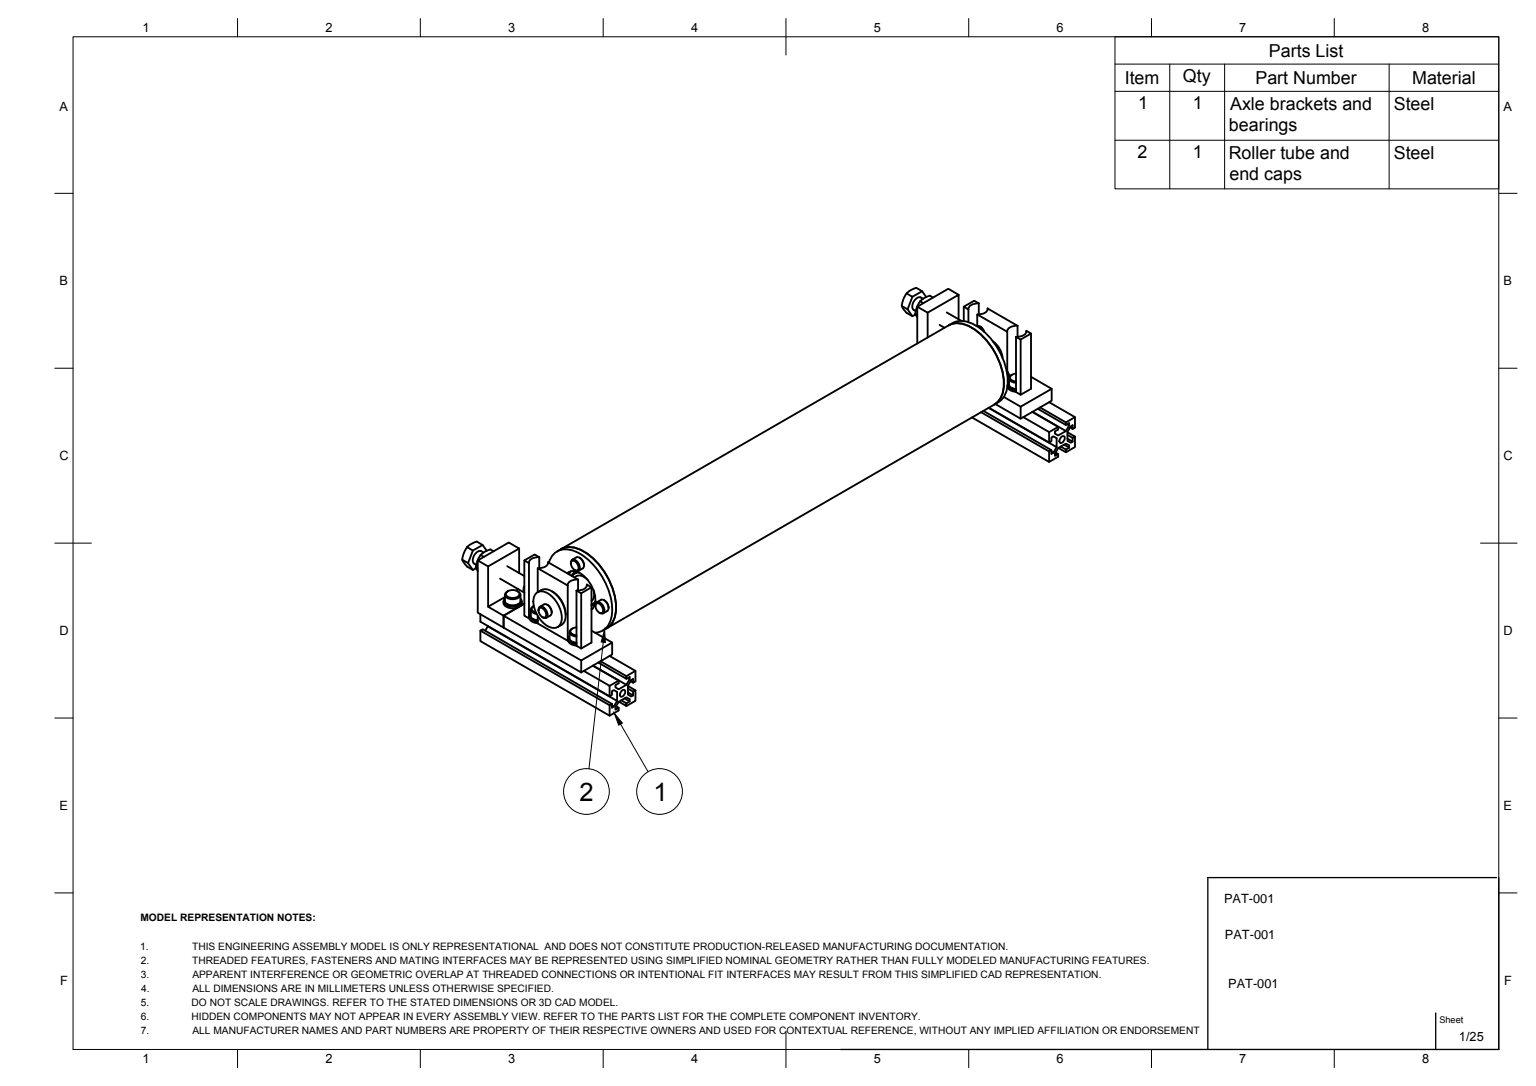
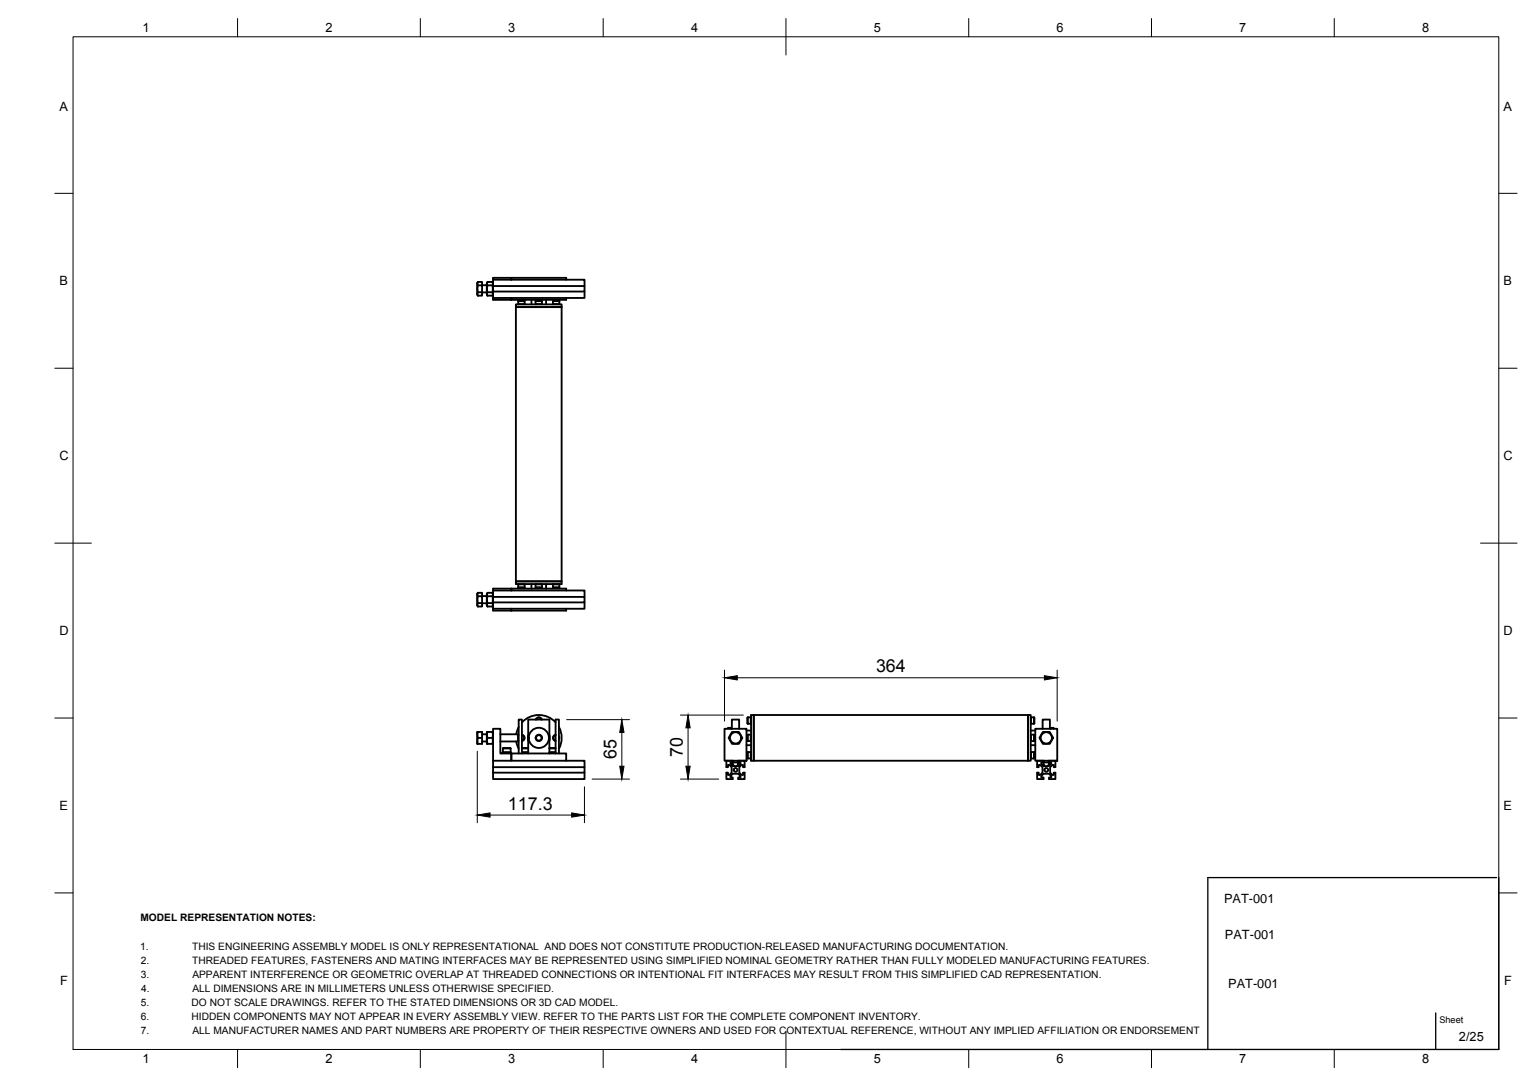
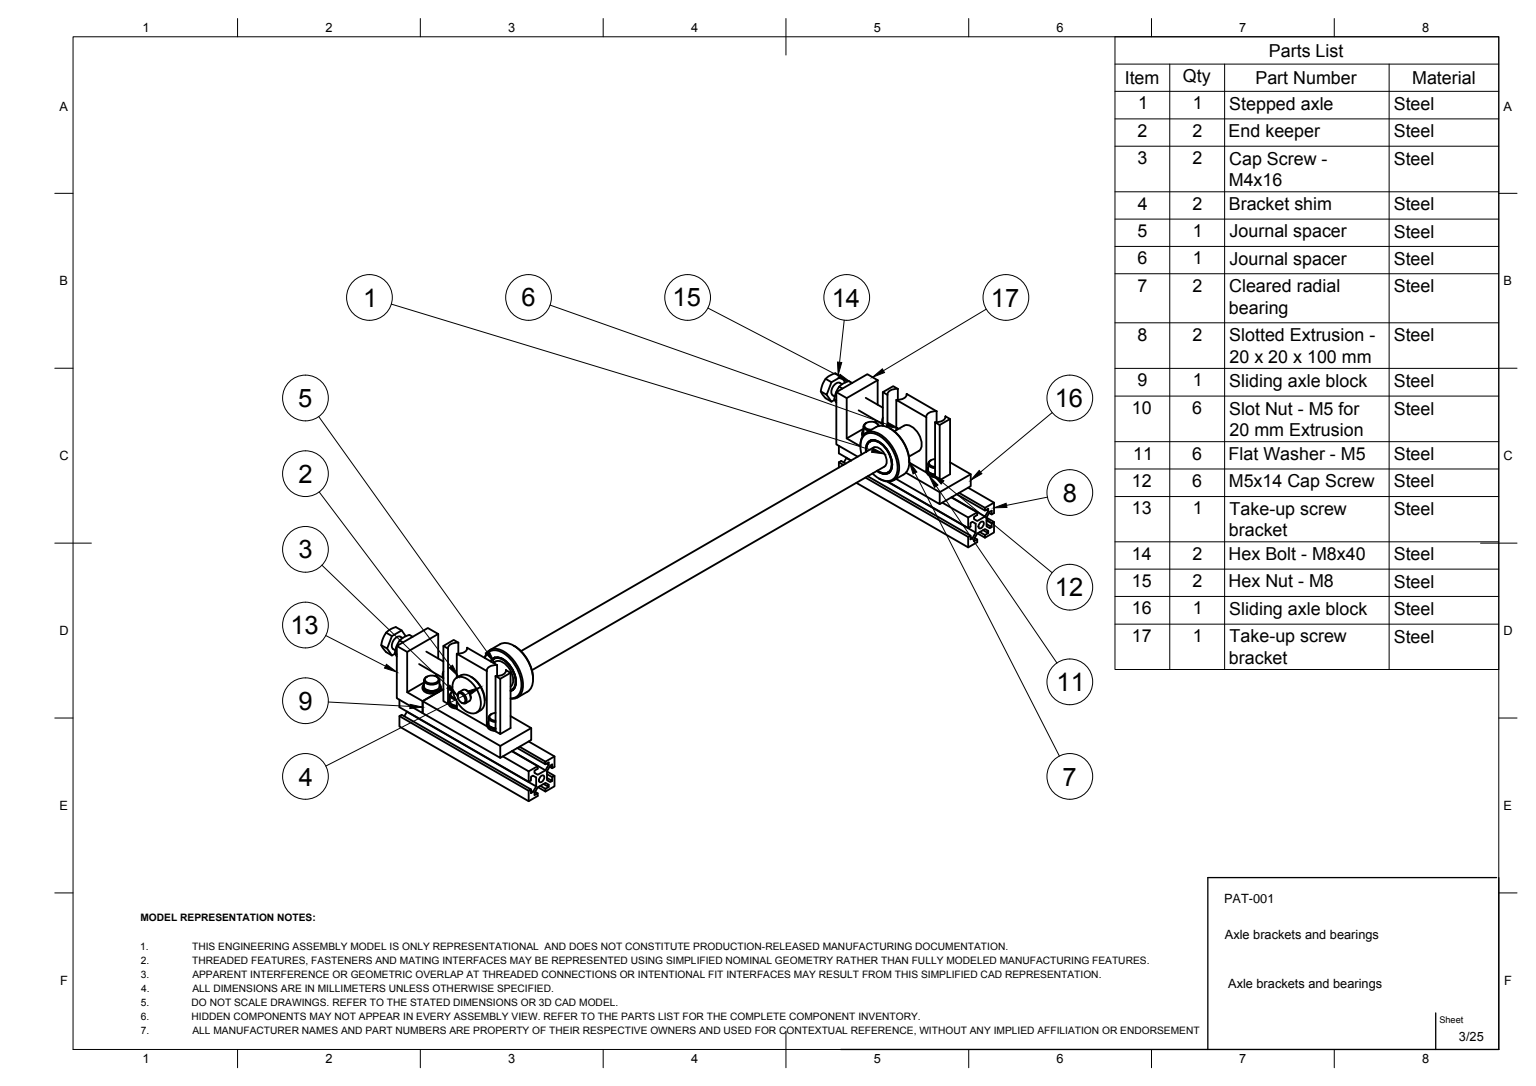
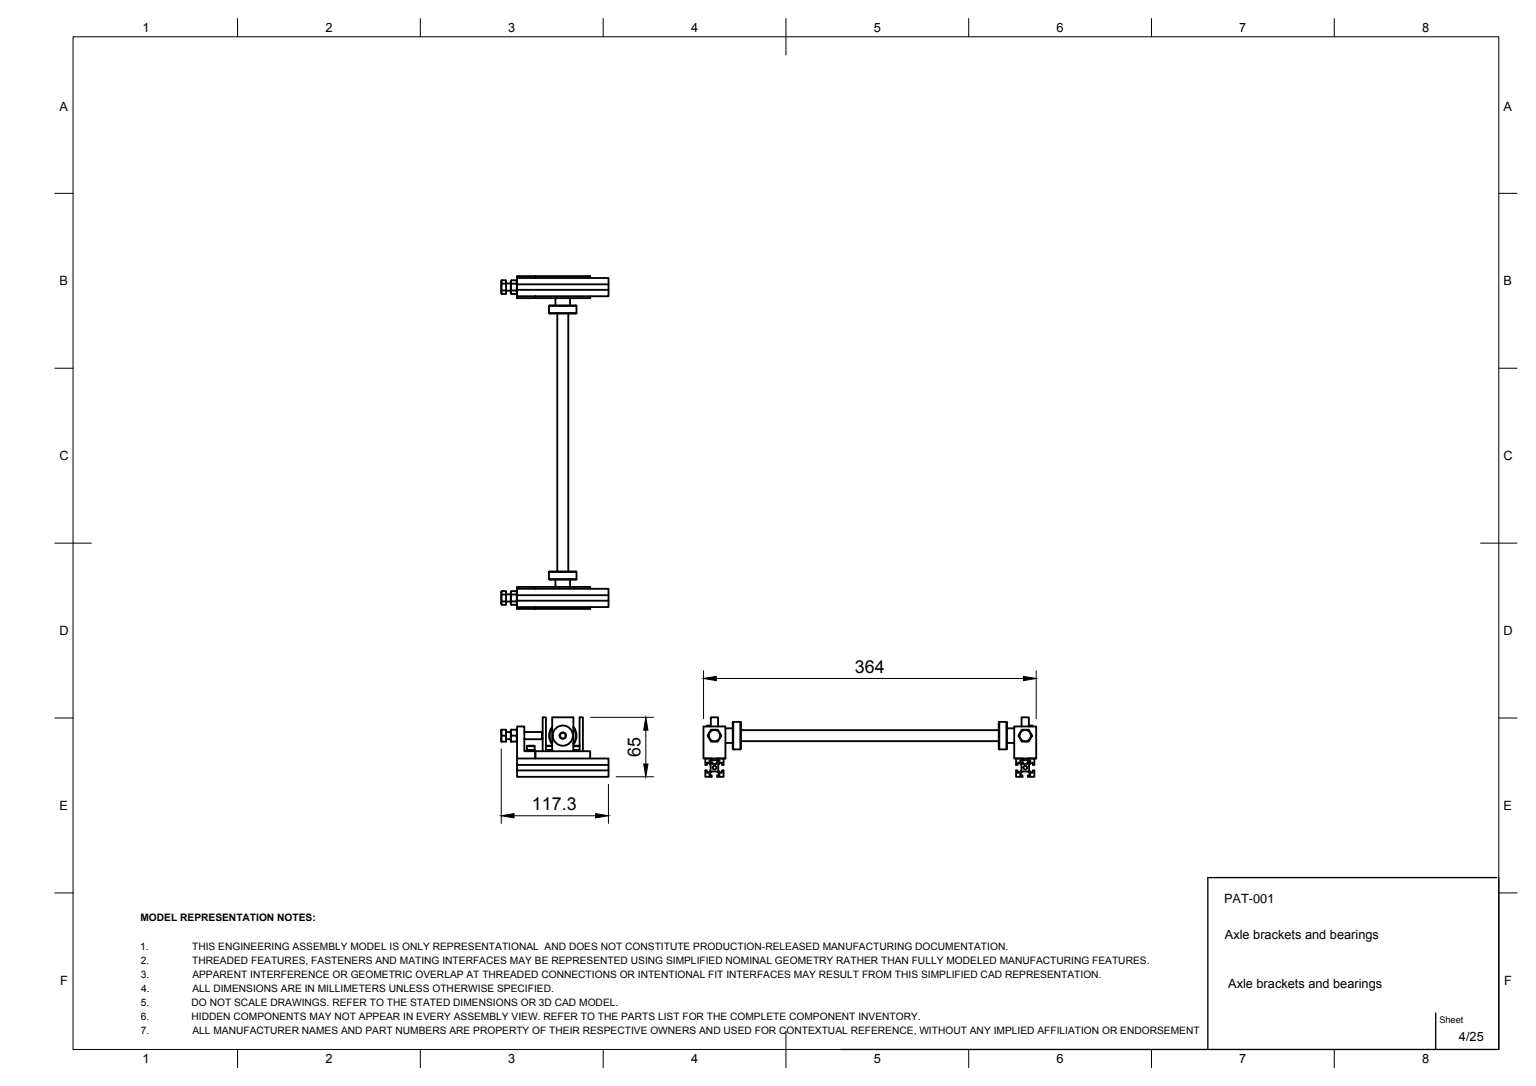
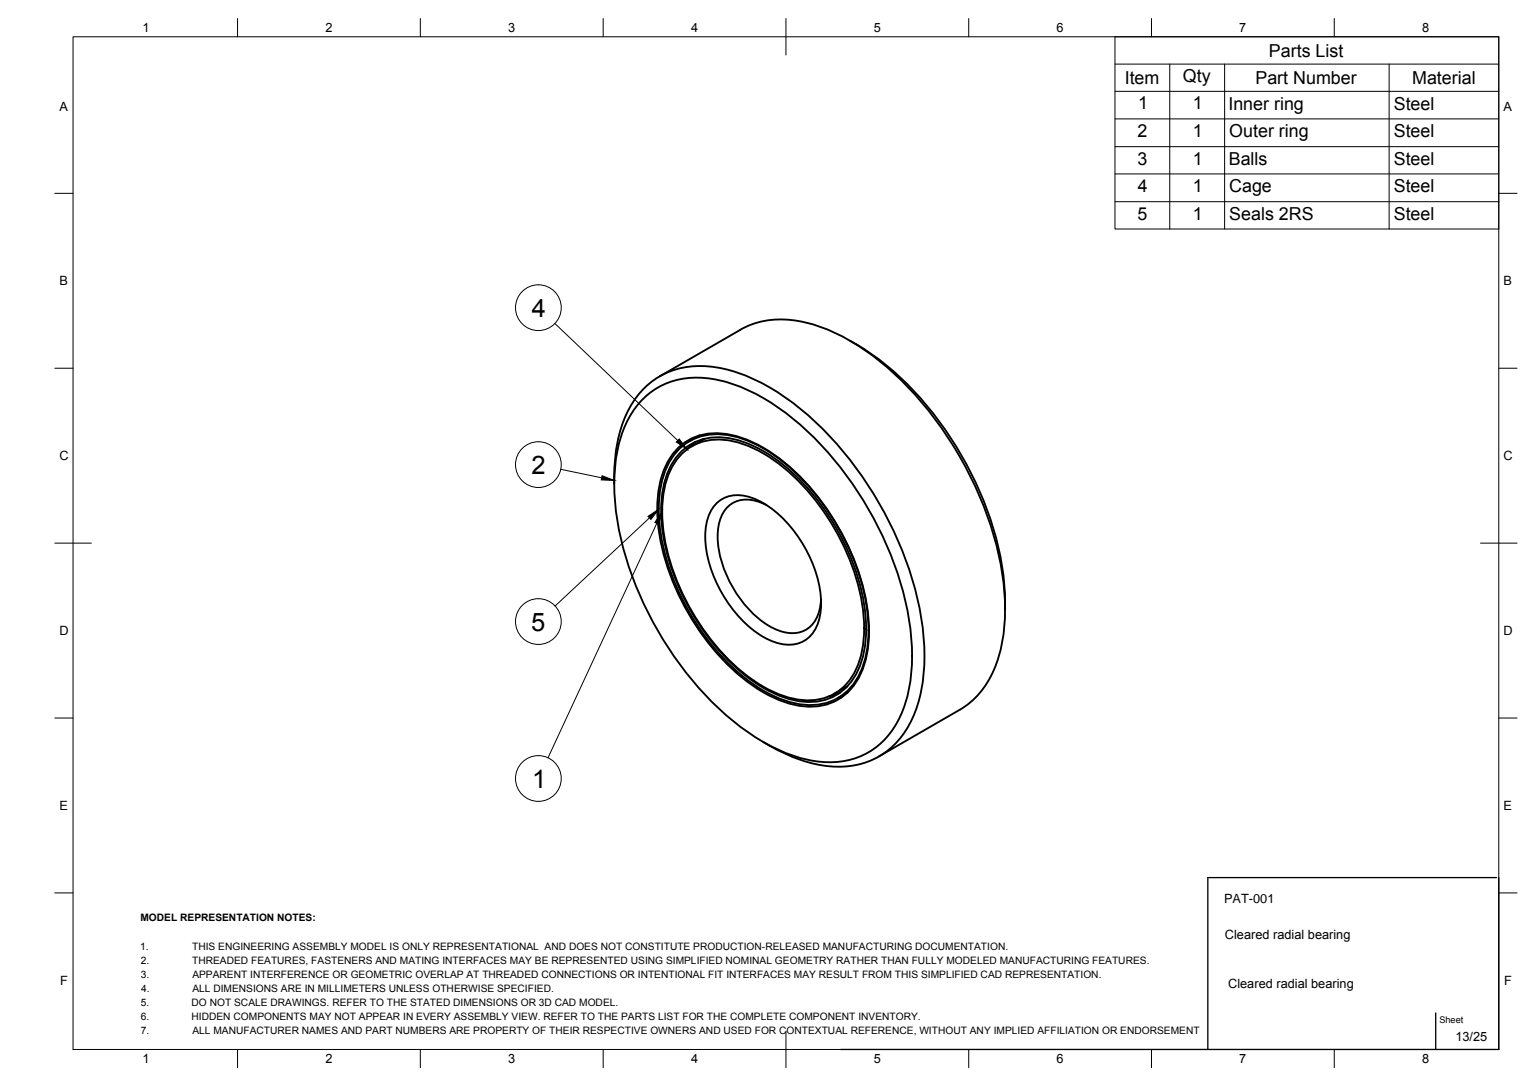
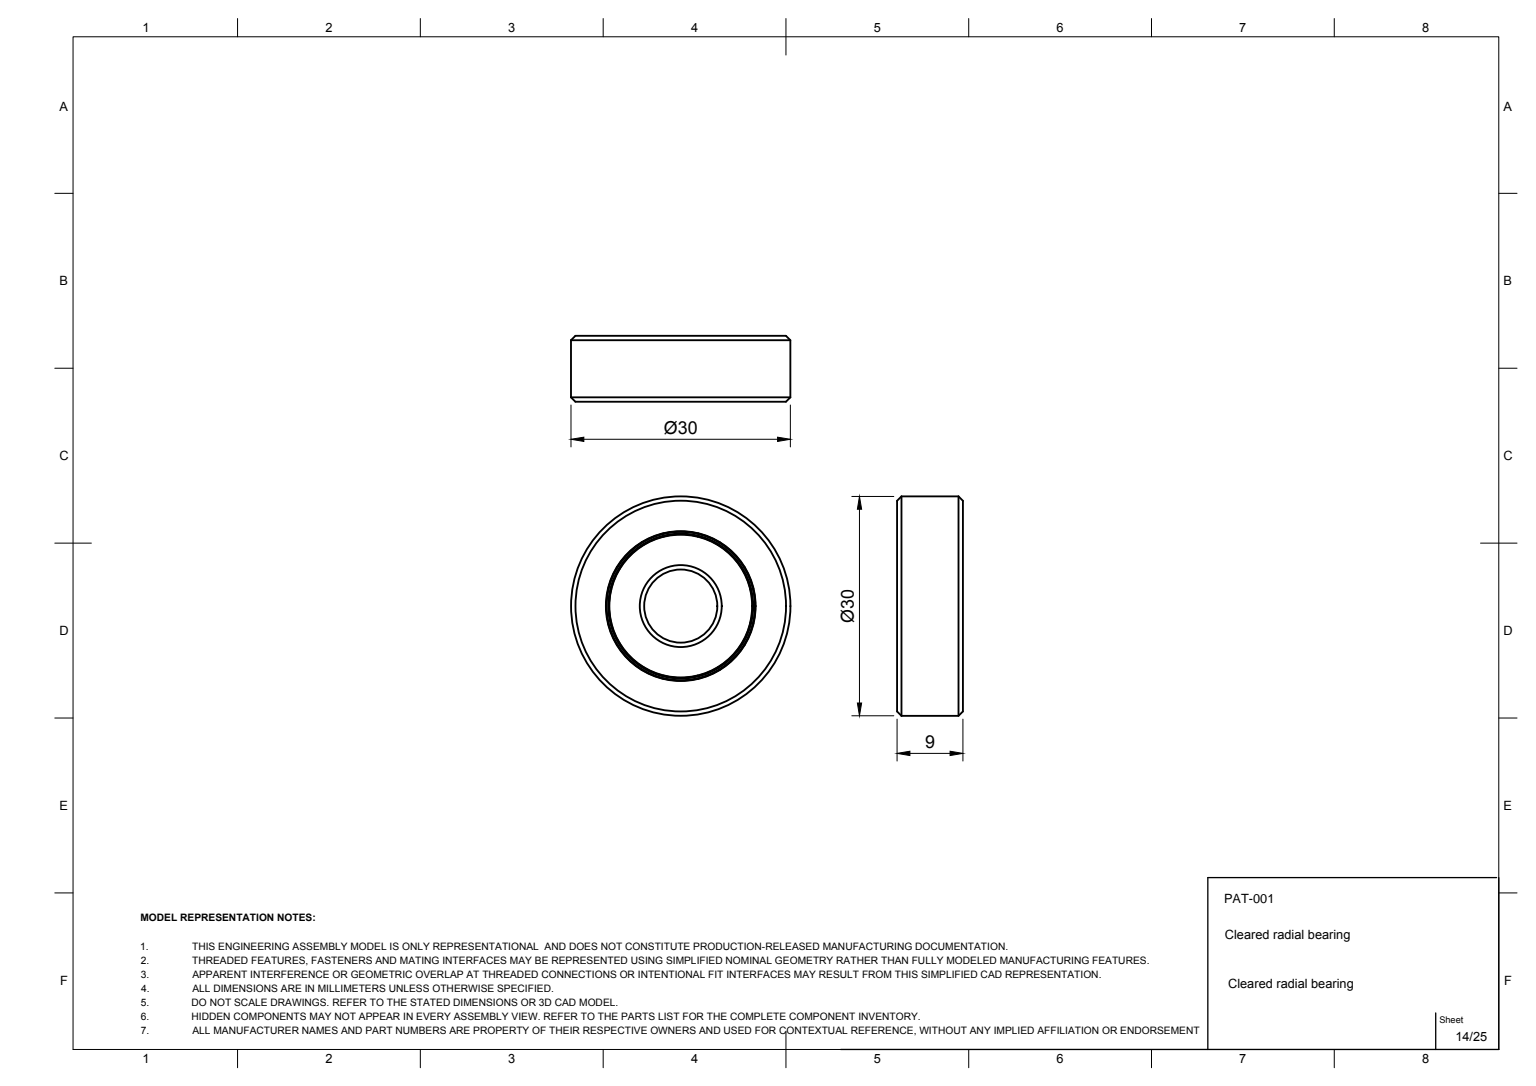
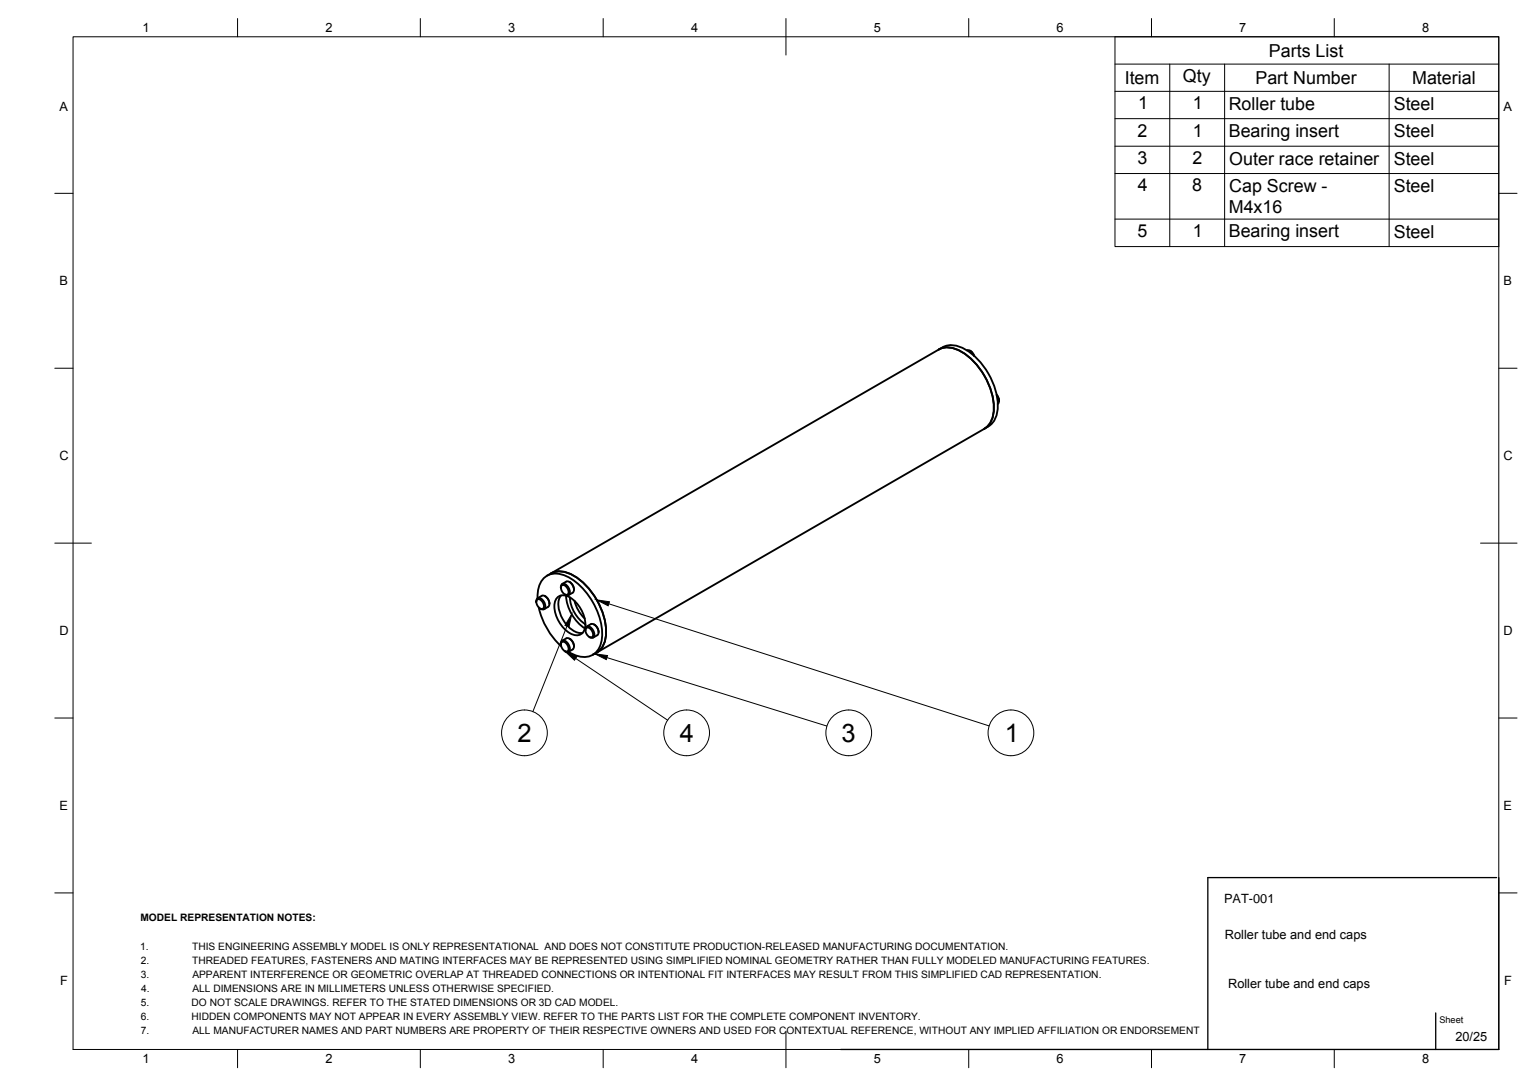
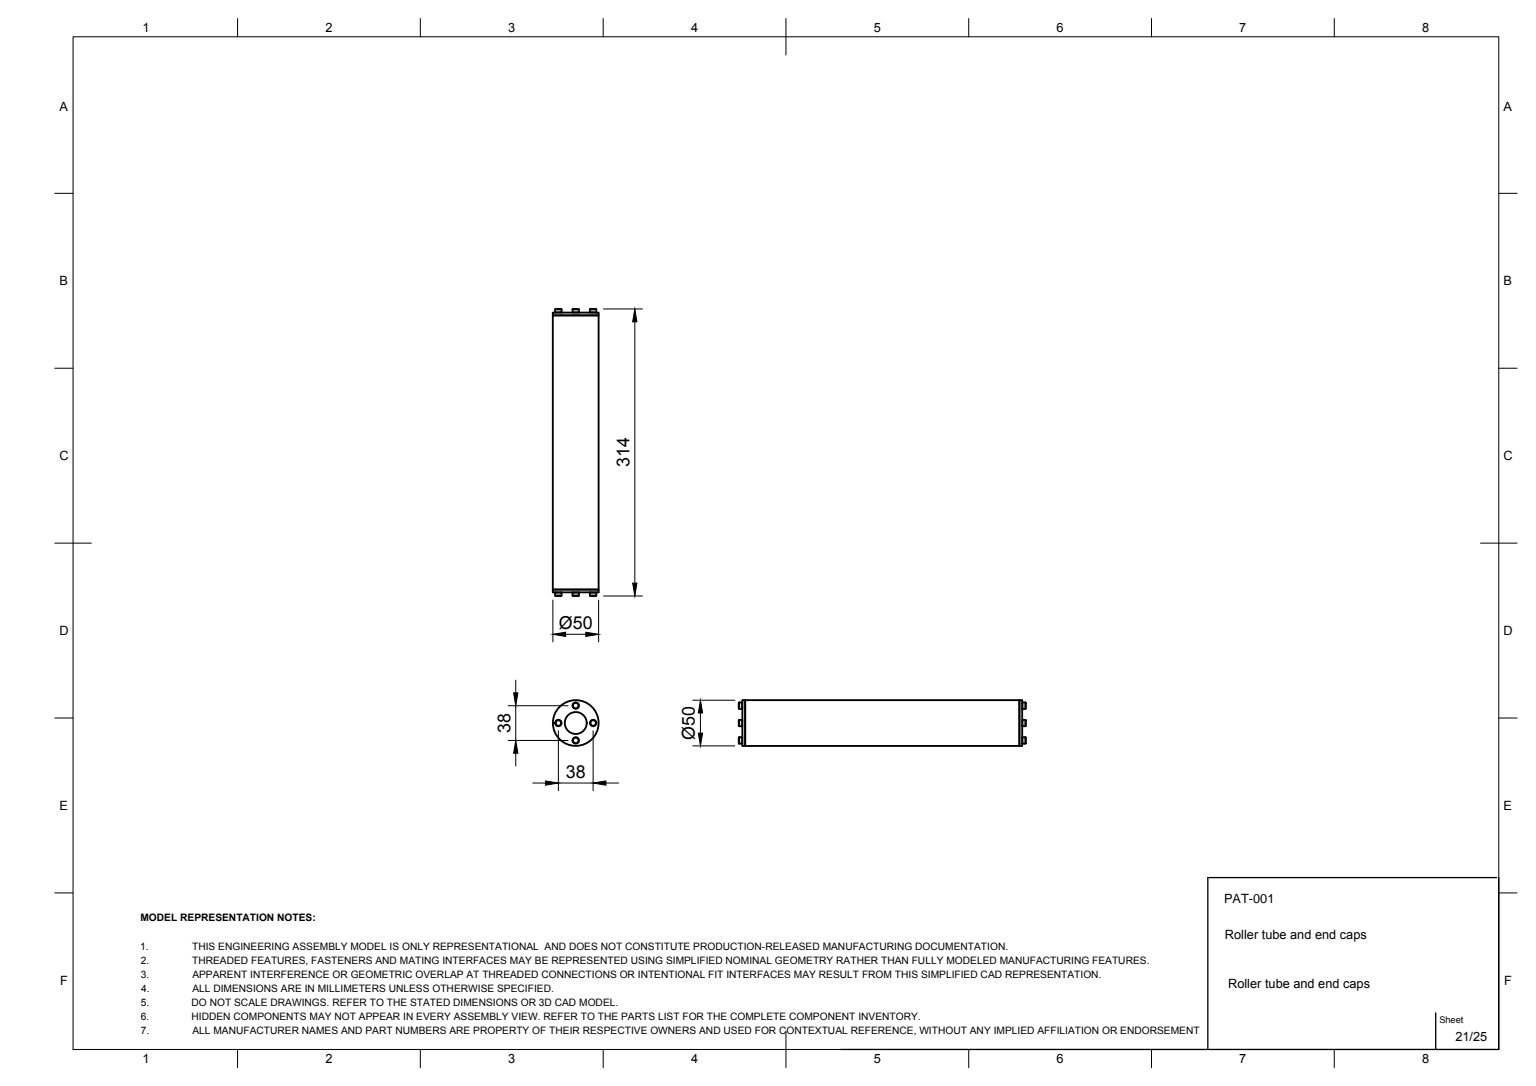
ISO-10303-21;
HEADER;
/* Generated by software containing ST-Developer
 * from STEP Tools, Inc. (www.steptools.com) 
 */

FILE_DESCRIPTION(
/* description */ ('PAT-001'),
/* implementation_level */ '2;1');

FILE_NAME(
/* name */ 'PAT-001',
/* time_stamp */ '2026-10-29T17:07:15-07:00',
/* author */ (''),
/* organization */ (''),
/* preprocessor_version */ 'ST-DEVELOPER v20.2',
/* originating_system */ 'Autodesk Translation Framework v15.17.0.0',
/* authorisation */ '');

FILE_SCHEMA (('AUTOMOTIVE_DESIGN { 1 0 10303 214 3 1 1 }'));
ENDSEC;

DATA;
#10=MECHANICAL_DESIGN_GEOMETRIC_PRESENTATION_REPRESENTATION('',(#373,#374,
#375,#376,#377,#378,#379,#380,#381,#382,#383,#384,#385,#386,#387,#388,#389,
#390,#391,#392,#393,#394,#395,#396,#397,#398,#399,#400,#401,#402,#403,#404,
#405),#9622);
#11=(
BOUNDED_CURVE()
B_SPLINE_CURVE(2,(#9167,#9168,#9169),.UNSPECIFIED.,.F.,.F.)
B_SPLINE_CURVE_WITH_KNOTS((3,3),(0.14973948338295,0.97160236658079),
 .UNSPECIFIED.)
CURVE()
GEOMETRIC_REPRESENTATION_ITEM()
RATIONAL_B_SPLINE_CURVE((1.07140024848292,1.23714644374248,1.07140024848292))
REPRESENTATION_ITEM('')
);
#12=(
BOUNDED_CURVE()
B_SPLINE_CURVE(2,(#9171,#9172,#9173),.UNSPECIFIED.,.F.,.F.)
B_SPLINE_CURVE_WITH_KNOTS((3,3),(0.14973948338295,0.97160236658079),
 .UNSPECIFIED.)
CURVE()
GEOMETRIC_REPRESENTATION_ITEM()
RATIONAL_B_SPLINE_CURVE((1.07140024848292,1.23714644374248,1.07140024848292))
REPRESENTATION_ITEM('')
);
#13=(
BOUNDED_CURVE()
B_SPLINE_CURVE(2,(#9175,#9176,#9177),.UNSPECIFIED.,.F.,.F.)
B_SPLINE_CURVE_WITH_KNOTS((3,3),(0.14973948338295,0.97160236658079),
 .UNSPECIFIED.)
CURVE()
GEOMETRIC_REPRESENTATION_ITEM()
RATIONAL_B_SPLINE_CURVE((1.07140024848292,1.23714644374248,1.07140024848292))
REPRESENTATION_ITEM('')
);
#14=(
BOUNDED_CURVE()
B_SPLINE_CURVE(2,(#9179,#9180,#9181),.UNSPECIFIED.,.F.,.F.)
B_SPLINE_CURVE_WITH_KNOTS((3,3),(0.149739483382949,0.971602366580789),
 .UNSPECIFIED.)
CURVE()
GEOMETRIC_REPRESENTATION_ITEM()
RATIONAL_B_SPLINE_CURVE((1.07140024848292,1.23714644374248,1.07140024848292))
REPRESENTATION_ITEM('')
);
#15=(
BOUNDED_CURVE()
B_SPLINE_CURVE(2,(#9183,#9184,#9185),.UNSPECIFIED.,.F.,.F.)
B_SPLINE_CURVE_WITH_KNOTS((3,3),(0.14973948338295,0.971602366580789),
 .UNSPECIFIED.)
CURVE()
GEOMETRIC_REPRESENTATION_ITEM()
RATIONAL_B_SPLINE_CURVE((1.07140024848292,1.23714644374248,1.07140024848292))
REPRESENTATION_ITEM('')
);
#16=(
BOUNDED_CURVE()
B_SPLINE_CURVE(2,(#9186,#9187,#9188),.UNSPECIFIED.,.F.,.F.)
B_SPLINE_CURVE_WITH_KNOTS((3,3),(0.14973948338295,0.97160236658079),
 .UNSPECIFIED.)
CURVE()
GEOMETRIC_REPRESENTATION_ITEM()
RATIONAL_B_SPLINE_CURVE((1.07140024848292,1.23714644374248,1.07140024848292))
REPRESENTATION_ITEM('')
);
#17=(
BOUNDED_CURVE()
B_SPLINE_CURVE(2,(#9219,#9220,#9221),.UNSPECIFIED.,.F.,.F.)
B_SPLINE_CURVE_WITH_KNOTS((3,3),(0.14973948338295,0.97160236658079),
 .UNSPECIFIED.)
CURVE()
GEOMETRIC_REPRESENTATION_ITEM()
RATIONAL_B_SPLINE_CURVE((1.07140024848292,1.23714644374248,1.07140024848292))
REPRESENTATION_ITEM('')
);
#18=(
BOUNDED_CURVE()
B_SPLINE_CURVE(2,(#9223,#9224,#9225),.UNSPECIFIED.,.F.,.F.)
B_SPLINE_CURVE_WITH_KNOTS((3,3),(0.14973948338295,0.971602366580789),
 .UNSPECIFIED.)
CURVE()
GEOMETRIC_REPRESENTATION_ITEM()
RATIONAL_B_SPLINE_CURVE((1.07140024848292,1.23714644374248,1.07140024848292))
REPRESENTATION_ITEM('')
);
#19=(
BOUNDED_CURVE()
B_SPLINE_CURVE(2,(#9230,#9231,#9232),.UNSPECIFIED.,.F.,.F.)
B_SPLINE_CURVE_WITH_KNOTS((3,3),(0.14973948338295,0.97160236658079),
 .UNSPECIFIED.)
CURVE()
GEOMETRIC_REPRESENTATION_ITEM()
RATIONAL_B_SPLINE_CURVE((1.07140024848292,1.23714644374248,1.07140024848292))
REPRESENTATION_ITEM('')
);
#20=(
BOUNDED_CURVE()
B_SPLINE_CURVE(2,(#9234,#9235,#9236),.UNSPECIFIED.,.F.,.F.)
B_SPLINE_CURVE_WITH_KNOTS((3,3),(0.14973948338295,0.97160236658079),
 .UNSPECIFIED.)
CURVE()
GEOMETRIC_REPRESENTATION_ITEM()
RATIONAL_B_SPLINE_CURVE((1.07140024848292,1.23714644374248,1.07140024848292))
REPRESENTATION_ITEM('')
);
#21=(
BOUNDED_CURVE()
B_SPLINE_CURVE(2,(#9238,#9239,#9240),.UNSPECIFIED.,.F.,.F.)
B_SPLINE_CURVE_WITH_KNOTS((3,3),(0.14973948338295,0.971602366580789),
 .UNSPECIFIED.)
CURVE()
GEOMETRIC_REPRESENTATION_ITEM()
RATIONAL_B_SPLINE_CURVE((1.07140024848292,1.23714644374248,1.07140024848292))
REPRESENTATION_ITEM('')
);
#22=(
BOUNDED_CURVE()
B_SPLINE_CURVE(2,(#9241,#9242,#9243),.UNSPECIFIED.,.F.,.F.)
B_SPLINE_CURVE_WITH_KNOTS((3,3),(0.14973948338295,0.97160236658079),
 .UNSPECIFIED.)
CURVE()
GEOMETRIC_REPRESENTATION_ITEM()
RATIONAL_B_SPLINE_CURVE((1.07140024848292,1.23714644374248,1.07140024848292))
REPRESENTATION_ITEM('')
);
#23=(
BOUNDED_CURVE()
B_SPLINE_CURVE(2,(#9250,#9251,#9252),.UNSPECIFIED.,.F.,.F.)
B_SPLINE_CURVE_WITH_KNOTS((3,3),(0.14973948338295,0.97160236658079),
 .UNSPECIFIED.)
CURVE()
GEOMETRIC_REPRESENTATION_ITEM()
RATIONAL_B_SPLINE_CURVE((1.07140024848292,1.23714644374248,1.07140024848292))
REPRESENTATION_ITEM('')
);
#24=(
BOUNDED_CURVE()
B_SPLINE_CURVE(2,(#9254,#9255,#9256),.UNSPECIFIED.,.F.,.F.)
B_SPLINE_CURVE_WITH_KNOTS((3,3),(0.14973948338295,0.97160236658079),
 .UNSPECIFIED.)
CURVE()
GEOMETRIC_REPRESENTATION_ITEM()
RATIONAL_B_SPLINE_CURVE((1.07140024848292,1.23714644374248,1.07140024848292))
REPRESENTATION_ITEM('')
);
#25=(
BOUNDED_CURVE()
B_SPLINE_CURVE(2,(#9258,#9259,#9260),.UNSPECIFIED.,.F.,.F.)
B_SPLINE_CURVE_WITH_KNOTS((3,3),(0.14973948338295,0.971602366580789),
 .UNSPECIFIED.)
CURVE()
GEOMETRIC_REPRESENTATION_ITEM()
RATIONAL_B_SPLINE_CURVE((1.07140024848292,1.23714644374248,1.07140024848292))
REPRESENTATION_ITEM('')
);
#26=(
BOUNDED_CURVE()
B_SPLINE_CURVE(2,(#9262,#9263,#9264),.UNSPECIFIED.,.F.,.F.)
B_SPLINE_CURVE_WITH_KNOTS((3,3),(0.14973948338295,0.97160236658079),
 .UNSPECIFIED.)
CURVE()
GEOMETRIC_REPRESENTATION_ITEM()
RATIONAL_B_SPLINE_CURVE((1.07140024848292,1.23714644374248,1.07140024848292))
REPRESENTATION_ITEM('')
);
#27=(
BOUNDED_CURVE()
B_SPLINE_CURVE(2,(#9266,#9267,#9268),.UNSPECIFIED.,.F.,.F.)
B_SPLINE_CURVE_WITH_KNOTS((3,3),(0.14973948338295,0.97160236658079),
 .UNSPECIFIED.)
CURVE()
GEOMETRIC_REPRESENTATION_ITEM()
RATIONAL_B_SPLINE_CURVE((1.07140024848292,1.23714644374248,1.07140024848292))
REPRESENTATION_ITEM('')
);
#28=(
BOUNDED_CURVE()
B_SPLINE_CURVE(2,(#9269,#9270,#9271),.UNSPECIFIED.,.F.,.F.)
B_SPLINE_CURVE_WITH_KNOTS((3,3),(0.14973948338295,0.971602366580789),
 .UNSPECIFIED.)
CURVE()
GEOMETRIC_REPRESENTATION_ITEM()
RATIONAL_B_SPLINE_CURVE((1.07140024848292,1.23714644374248,1.07140024848292))
REPRESENTATION_ITEM('')
);
#29=ORIENTED_CLOSED_SHELL('',*,#5223,.F.);
#30=ORIENTED_CLOSED_SHELL('',*,#5232,.F.);
#31=BREP_WITH_VOIDS('Body1',#5224,(#29));
#32=BREP_WITH_VOIDS('Body1',#5231,(#30));
#33=ELLIPSE('',#5863,0.299389011154384,0.2117);
#34=ELLIPSE('',#5868,0.299389011154384,0.2117);
#35=ITEM_DEFINED_TRANSFORMATION($,$,#5570,#5698);
#36=ITEM_DEFINED_TRANSFORMATION($,$,#5590,#5699);
#37=ITEM_DEFINED_TRANSFORMATION($,$,#5610,#5700);
#38=ITEM_DEFINED_TRANSFORMATION($,$,#5627,#5701);
#39=ITEM_DEFINED_TRANSFORMATION($,$,#5681,#5702);
#40=ITEM_DEFINED_TRANSFORMATION($,$,#5511,#6053);
#41=ITEM_DEFINED_TRANSFORMATION($,$,#5533,#6054);
#42=ITEM_DEFINED_TRANSFORMATION($,$,#5542,#6055);
#43=ITEM_DEFINED_TRANSFORMATION($,$,#5551,#6056);
#44=ITEM_DEFINED_TRANSFORMATION($,$,#5551,#6057);
#45=ITEM_DEFINED_TRANSFORMATION($,$,#6027,#6058);
#46=ITEM_DEFINED_TRANSFORMATION($,$,#6027,#6059);
#47=ITEM_DEFINED_TRANSFORMATION($,$,#5560,#6060);
#48=ITEM_DEFINED_TRANSFORMATION($,$,#5560,#6061);
#49=ITEM_DEFINED_TRANSFORMATION($,$,#5569,#6062);
#50=ITEM_DEFINED_TRANSFORMATION($,$,#5569,#6063);
#51=ITEM_DEFINED_TRANSFORMATION($,$,#5703,#6064);
#52=ITEM_DEFINED_TRANSFORMATION($,$,#5742,#6065);
#53=ITEM_DEFINED_TRANSFORMATION($,$,#5757,#6066);
#54=ITEM_DEFINED_TRANSFORMATION($,$,#5796,#6067);
#55=ITEM_DEFINED_TRANSFORMATION($,$,#5811,#6068);
#56=ITEM_DEFINED_TRANSFORMATION($,$,#5861,#6069);
#57=ITEM_DEFINED_TRANSFORMATION($,$,#5878,#6070);
#58=ITEM_DEFINED_TRANSFORMATION($,$,#5889,#6071);
#59=ITEM_DEFINED_TRANSFORMATION($,$,#5861,#6072);
#60=ITEM_DEFINED_TRANSFORMATION($,$,#5878,#6073);
#61=ITEM_DEFINED_TRANSFORMATION($,$,#5889,#6074);
#62=ITEM_DEFINED_TRANSFORMATION($,$,#5861,#6075);
#63=ITEM_DEFINED_TRANSFORMATION($,$,#5878,#6076);
#64=ITEM_DEFINED_TRANSFORMATION($,$,#5889,#6077);
#65=ITEM_DEFINED_TRANSFORMATION($,$,#5913,#6078);
#66=ITEM_DEFINED_TRANSFORMATION($,$,#5930,#6079);
#67=ITEM_DEFINED_TRANSFORMATION($,$,#5811,#6080);
#68=ITEM_DEFINED_TRANSFORMATION($,$,#5861,#6081);
#69=ITEM_DEFINED_TRANSFORMATION($,$,#5878,#6082);
#70=ITEM_DEFINED_TRANSFORMATION($,$,#5889,#6083);
#71=ITEM_DEFINED_TRANSFORMATION($,$,#5861,#6084);
#72=ITEM_DEFINED_TRANSFORMATION($,$,#5878,#6085);
#73=ITEM_DEFINED_TRANSFORMATION($,$,#5889,#6086);
#74=ITEM_DEFINED_TRANSFORMATION($,$,#5861,#6087);
#75=ITEM_DEFINED_TRANSFORMATION($,$,#5878,#6088);
#76=ITEM_DEFINED_TRANSFORMATION($,$,#5889,#6089);
#77=ITEM_DEFINED_TRANSFORMATION($,$,#5913,#6090);
#78=ITEM_DEFINED_TRANSFORMATION($,$,#5930,#6091);
#79=ITEM_DEFINED_TRANSFORMATION($,$,#5947,#6092);
#80=ITEM_DEFINED_TRANSFORMATION($,$,#5972,#6093);
#81=ITEM_DEFINED_TRANSFORMATION($,$,#5997,#6094);
#82=ITEM_DEFINED_TRANSFORMATION($,$,#6006,#6095);
#83=ITEM_DEFINED_TRANSFORMATION($,$,#6027,#6096);
#84=ITEM_DEFINED_TRANSFORMATION($,$,#6027,#6097);
#85=ITEM_DEFINED_TRANSFORMATION($,$,#6027,#6098);
#86=ITEM_DEFINED_TRANSFORMATION($,$,#6027,#6099);
#87=ITEM_DEFINED_TRANSFORMATION($,$,#6006,#6100);
#88=ITEM_DEFINED_TRANSFORMATION($,$,#6027,#6101);
#89=ITEM_DEFINED_TRANSFORMATION($,$,#6027,#6102);
#90=ITEM_DEFINED_TRANSFORMATION($,$,#6027,#6103);
#91=ITEM_DEFINED_TRANSFORMATION($,$,#6027,#6104);
#92=ITEM_DEFINED_TRANSFORMATION($,$,#5510,#6105);
#93=ITEM_DEFINED_TRANSFORMATION($,$,#5946,#6106);
#94=(
REPRESENTATION_RELATIONSHIP($,$,#9752,#9751)
REPRESENTATION_RELATIONSHIP_WITH_TRANSFORMATION(#35)
SHAPE_REPRESENTATION_RELATIONSHIP()
);
#95=(
REPRESENTATION_RELATIONSHIP($,$,#9753,#9751)
REPRESENTATION_RELATIONSHIP_WITH_TRANSFORMATION(#36)
SHAPE_REPRESENTATION_RELATIONSHIP()
);
#96=(
REPRESENTATION_RELATIONSHIP($,$,#9754,#9751)
REPRESENTATION_RELATIONSHIP_WITH_TRANSFORMATION(#37)
SHAPE_REPRESENTATION_RELATIONSHIP()
);
#97=(
REPRESENTATION_RELATIONSHIP($,$,#9755,#9751)
REPRESENTATION_RELATIONSHIP_WITH_TRANSFORMATION(#38)
SHAPE_REPRESENTATION_RELATIONSHIP()
);
#98=(
REPRESENTATION_RELATIONSHIP($,$,#9756,#9751)
REPRESENTATION_RELATIONSHIP_WITH_TRANSFORMATION(#39)
SHAPE_REPRESENTATION_RELATIONSHIP()
);
#99=(
REPRESENTATION_RELATIONSHIP($,$,#9746,#9745)
REPRESENTATION_RELATIONSHIP_WITH_TRANSFORMATION(#40)
SHAPE_REPRESENTATION_RELATIONSHIP()
);
#100=(
REPRESENTATION_RELATIONSHIP($,$,#9747,#9745)
REPRESENTATION_RELATIONSHIP_WITH_TRANSFORMATION(#41)
SHAPE_REPRESENTATION_RELATIONSHIP()
);
#101=(
REPRESENTATION_RELATIONSHIP($,$,#9748,#9745)
REPRESENTATION_RELATIONSHIP_WITH_TRANSFORMATION(#42)
SHAPE_REPRESENTATION_RELATIONSHIP()
);
#102=(
REPRESENTATION_RELATIONSHIP($,$,#9749,#9745)
REPRESENTATION_RELATIONSHIP_WITH_TRANSFORMATION(#43)
SHAPE_REPRESENTATION_RELATIONSHIP()
);
#103=(
REPRESENTATION_RELATIONSHIP($,$,#9749,#9745)
REPRESENTATION_RELATIONSHIP_WITH_TRANSFORMATION(#44)
SHAPE_REPRESENTATION_RELATIONSHIP()
);
#104=(
REPRESENTATION_RELATIONSHIP($,$,#9772,#9745)
REPRESENTATION_RELATIONSHIP_WITH_TRANSFORMATION(#45)
SHAPE_REPRESENTATION_RELATIONSHIP()
);
#105=(
REPRESENTATION_RELATIONSHIP($,$,#9772,#9745)
REPRESENTATION_RELATIONSHIP_WITH_TRANSFORMATION(#46)
SHAPE_REPRESENTATION_RELATIONSHIP()
);
#106=(
REPRESENTATION_RELATIONSHIP($,$,#9750,#9745)
REPRESENTATION_RELATIONSHIP_WITH_TRANSFORMATION(#47)
SHAPE_REPRESENTATION_RELATIONSHIP()
);
#107=(
REPRESENTATION_RELATIONSHIP($,$,#9750,#9745)
REPRESENTATION_RELATIONSHIP_WITH_TRANSFORMATION(#48)
SHAPE_REPRESENTATION_RELATIONSHIP()
);
#108=(
REPRESENTATION_RELATIONSHIP($,$,#9751,#9745)
REPRESENTATION_RELATIONSHIP_WITH_TRANSFORMATION(#49)
SHAPE_REPRESENTATION_RELATIONSHIP()
);
#109=(
REPRESENTATION_RELATIONSHIP($,$,#9751,#9745)
REPRESENTATION_RELATIONSHIP_WITH_TRANSFORMATION(#50)
SHAPE_REPRESENTATION_RELATIONSHIP()
);
#110=(
REPRESENTATION_RELATIONSHIP($,$,#9757,#9745)
REPRESENTATION_RELATIONSHIP_WITH_TRANSFORMATION(#51)
SHAPE_REPRESENTATION_RELATIONSHIP()
);
#111=(
REPRESENTATION_RELATIONSHIP($,$,#9758,#9745)
REPRESENTATION_RELATIONSHIP_WITH_TRANSFORMATION(#52)
SHAPE_REPRESENTATION_RELATIONSHIP()
);
#112=(
REPRESENTATION_RELATIONSHIP($,$,#9759,#9745)
REPRESENTATION_RELATIONSHIP_WITH_TRANSFORMATION(#53)
SHAPE_REPRESENTATION_RELATIONSHIP()
);
#113=(
REPRESENTATION_RELATIONSHIP($,$,#9760,#9745)
REPRESENTATION_RELATIONSHIP_WITH_TRANSFORMATION(#54)
SHAPE_REPRESENTATION_RELATIONSHIP()
);
#114=(
REPRESENTATION_RELATIONSHIP($,$,#9761,#9745)
REPRESENTATION_RELATIONSHIP_WITH_TRANSFORMATION(#55)
SHAPE_REPRESENTATION_RELATIONSHIP()
);
#115=(
REPRESENTATION_RELATIONSHIP($,$,#9762,#9745)
REPRESENTATION_RELATIONSHIP_WITH_TRANSFORMATION(#56)
SHAPE_REPRESENTATION_RELATIONSHIP()
);
#116=(
REPRESENTATION_RELATIONSHIP($,$,#9763,#9745)
REPRESENTATION_RELATIONSHIP_WITH_TRANSFORMATION(#57)
SHAPE_REPRESENTATION_RELATIONSHIP()
);
#117=(
REPRESENTATION_RELATIONSHIP($,$,#9764,#9745)
REPRESENTATION_RELATIONSHIP_WITH_TRANSFORMATION(#58)
SHAPE_REPRESENTATION_RELATIONSHIP()
);
#118=(
REPRESENTATION_RELATIONSHIP($,$,#9762,#9745)
REPRESENTATION_RELATIONSHIP_WITH_TRANSFORMATION(#59)
SHAPE_REPRESENTATION_RELATIONSHIP()
);
#119=(
REPRESENTATION_RELATIONSHIP($,$,#9763,#9745)
REPRESENTATION_RELATIONSHIP_WITH_TRANSFORMATION(#60)
SHAPE_REPRESENTATION_RELATIONSHIP()
);
#120=(
REPRESENTATION_RELATIONSHIP($,$,#9764,#9745)
REPRESENTATION_RELATIONSHIP_WITH_TRANSFORMATION(#61)
SHAPE_REPRESENTATION_RELATIONSHIP()
);
#121=(
REPRESENTATION_RELATIONSHIP($,$,#9762,#9745)
REPRESENTATION_RELATIONSHIP_WITH_TRANSFORMATION(#62)
SHAPE_REPRESENTATION_RELATIONSHIP()
);
#122=(
REPRESENTATION_RELATIONSHIP($,$,#9763,#9745)
REPRESENTATION_RELATIONSHIP_WITH_TRANSFORMATION(#63)
SHAPE_REPRESENTATION_RELATIONSHIP()
);
#123=(
REPRESENTATION_RELATIONSHIP($,$,#9764,#9745)
REPRESENTATION_RELATIONSHIP_WITH_TRANSFORMATION(#64)
SHAPE_REPRESENTATION_RELATIONSHIP()
);
#124=(
REPRESENTATION_RELATIONSHIP($,$,#9765,#9745)
REPRESENTATION_RELATIONSHIP_WITH_TRANSFORMATION(#65)
SHAPE_REPRESENTATION_RELATIONSHIP()
);
#125=(
REPRESENTATION_RELATIONSHIP($,$,#9766,#9745)
REPRESENTATION_RELATIONSHIP_WITH_TRANSFORMATION(#66)
SHAPE_REPRESENTATION_RELATIONSHIP()
);
#126=(
REPRESENTATION_RELATIONSHIP($,$,#9761,#9745)
REPRESENTATION_RELATIONSHIP_WITH_TRANSFORMATION(#67)
SHAPE_REPRESENTATION_RELATIONSHIP()
);
#127=(
REPRESENTATION_RELATIONSHIP($,$,#9762,#9745)
REPRESENTATION_RELATIONSHIP_WITH_TRANSFORMATION(#68)
SHAPE_REPRESENTATION_RELATIONSHIP()
);
#128=(
REPRESENTATION_RELATIONSHIP($,$,#9763,#9745)
REPRESENTATION_RELATIONSHIP_WITH_TRANSFORMATION(#69)
SHAPE_REPRESENTATION_RELATIONSHIP()
);
#129=(
REPRESENTATION_RELATIONSHIP($,$,#9764,#9745)
REPRESENTATION_RELATIONSHIP_WITH_TRANSFORMATION(#70)
SHAPE_REPRESENTATION_RELATIONSHIP()
);
#130=(
REPRESENTATION_RELATIONSHIP($,$,#9762,#9745)
REPRESENTATION_RELATIONSHIP_WITH_TRANSFORMATION(#71)
SHAPE_REPRESENTATION_RELATIONSHIP()
);
#131=(
REPRESENTATION_RELATIONSHIP($,$,#9763,#9745)
REPRESENTATION_RELATIONSHIP_WITH_TRANSFORMATION(#72)
SHAPE_REPRESENTATION_RELATIONSHIP()
);
#132=(
REPRESENTATION_RELATIONSHIP($,$,#9764,#9745)
REPRESENTATION_RELATIONSHIP_WITH_TRANSFORMATION(#73)
SHAPE_REPRESENTATION_RELATIONSHIP()
);
#133=(
REPRESENTATION_RELATIONSHIP($,$,#9762,#9745)
REPRESENTATION_RELATIONSHIP_WITH_TRANSFORMATION(#74)
SHAPE_REPRESENTATION_RELATIONSHIP()
);
#134=(
REPRESENTATION_RELATIONSHIP($,$,#9763,#9745)
REPRESENTATION_RELATIONSHIP_WITH_TRANSFORMATION(#75)
SHAPE_REPRESENTATION_RELATIONSHIP()
);
#135=(
REPRESENTATION_RELATIONSHIP($,$,#9764,#9745)
REPRESENTATION_RELATIONSHIP_WITH_TRANSFORMATION(#76)
SHAPE_REPRESENTATION_RELATIONSHIP()
);
#136=(
REPRESENTATION_RELATIONSHIP($,$,#9765,#9745)
REPRESENTATION_RELATIONSHIP_WITH_TRANSFORMATION(#77)
SHAPE_REPRESENTATION_RELATIONSHIP()
);
#137=(
REPRESENTATION_RELATIONSHIP($,$,#9766,#9745)
REPRESENTATION_RELATIONSHIP_WITH_TRANSFORMATION(#78)
SHAPE_REPRESENTATION_RELATIONSHIP()
);
#138=(
REPRESENTATION_RELATIONSHIP($,$,#9768,#9767)
REPRESENTATION_RELATIONSHIP_WITH_TRANSFORMATION(#79)
SHAPE_REPRESENTATION_RELATIONSHIP()
);
#139=(
REPRESENTATION_RELATIONSHIP($,$,#9769,#9767)
REPRESENTATION_RELATIONSHIP_WITH_TRANSFORMATION(#80)
SHAPE_REPRESENTATION_RELATIONSHIP()
);
#140=(
REPRESENTATION_RELATIONSHIP($,$,#9770,#9767)
REPRESENTATION_RELATIONSHIP_WITH_TRANSFORMATION(#81)
SHAPE_REPRESENTATION_RELATIONSHIP()
);
#141=(
REPRESENTATION_RELATIONSHIP($,$,#9771,#9767)
REPRESENTATION_RELATIONSHIP_WITH_TRANSFORMATION(#82)
SHAPE_REPRESENTATION_RELATIONSHIP()
);
#142=(
REPRESENTATION_RELATIONSHIP($,$,#9772,#9767)
REPRESENTATION_RELATIONSHIP_WITH_TRANSFORMATION(#83)
SHAPE_REPRESENTATION_RELATIONSHIP()
);
#143=(
REPRESENTATION_RELATIONSHIP($,$,#9772,#9767)
REPRESENTATION_RELATIONSHIP_WITH_TRANSFORMATION(#84)
SHAPE_REPRESENTATION_RELATIONSHIP()
);
#144=(
REPRESENTATION_RELATIONSHIP($,$,#9772,#9767)
REPRESENTATION_RELATIONSHIP_WITH_TRANSFORMATION(#85)
SHAPE_REPRESENTATION_RELATIONSHIP()
);
#145=(
REPRESENTATION_RELATIONSHIP($,$,#9772,#9767)
REPRESENTATION_RELATIONSHIP_WITH_TRANSFORMATION(#86)
SHAPE_REPRESENTATION_RELATIONSHIP()
);
#146=(
REPRESENTATION_RELATIONSHIP($,$,#9771,#9767)
REPRESENTATION_RELATIONSHIP_WITH_TRANSFORMATION(#87)
SHAPE_REPRESENTATION_RELATIONSHIP()
);
#147=(
REPRESENTATION_RELATIONSHIP($,$,#9772,#9767)
REPRESENTATION_RELATIONSHIP_WITH_TRANSFORMATION(#88)
SHAPE_REPRESENTATION_RELATIONSHIP()
);
#148=(
REPRESENTATION_RELATIONSHIP($,$,#9772,#9767)
REPRESENTATION_RELATIONSHIP_WITH_TRANSFORMATION(#89)
SHAPE_REPRESENTATION_RELATIONSHIP()
);
#149=(
REPRESENTATION_RELATIONSHIP($,$,#9772,#9767)
REPRESENTATION_RELATIONSHIP_WITH_TRANSFORMATION(#90)
SHAPE_REPRESENTATION_RELATIONSHIP()
);
#150=(
REPRESENTATION_RELATIONSHIP($,$,#9772,#9767)
REPRESENTATION_RELATIONSHIP_WITH_TRANSFORMATION(#91)
SHAPE_REPRESENTATION_RELATIONSHIP()
);
#151=(
REPRESENTATION_RELATIONSHIP($,$,#9745,#9744)
REPRESENTATION_RELATIONSHIP_WITH_TRANSFORMATION(#92)
SHAPE_REPRESENTATION_RELATIONSHIP()
);
#152=(
REPRESENTATION_RELATIONSHIP($,$,#9767,#9744)
REPRESENTATION_RELATIONSHIP_WITH_TRANSFORMATION(#93)
SHAPE_REPRESENTATION_RELATIONSHIP()
);
#153=CONTEXT_DEPENDENT_SHAPE_REPRESENTATION(#94,#9669);
#154=CONTEXT_DEPENDENT_SHAPE_REPRESENTATION(#95,#9670);
#155=CONTEXT_DEPENDENT_SHAPE_REPRESENTATION(#96,#9671);
#156=CONTEXT_DEPENDENT_SHAPE_REPRESENTATION(#97,#9672);
#157=CONTEXT_DEPENDENT_SHAPE_REPRESENTATION(#98,#9673);
#158=CONTEXT_DEPENDENT_SHAPE_REPRESENTATION(#99,#9690);
#159=CONTEXT_DEPENDENT_SHAPE_REPRESENTATION(#100,#9691);
#160=CONTEXT_DEPENDENT_SHAPE_REPRESENTATION(#101,#9692);
#161=CONTEXT_DEPENDENT_SHAPE_REPRESENTATION(#102,#9693);
#162=CONTEXT_DEPENDENT_SHAPE_REPRESENTATION(#103,#9694);
#163=CONTEXT_DEPENDENT_SHAPE_REPRESENTATION(#104,#9695);
#164=CONTEXT_DEPENDENT_SHAPE_REPRESENTATION(#105,#9696);
#165=CONTEXT_DEPENDENT_SHAPE_REPRESENTATION(#106,#9697);
#166=CONTEXT_DEPENDENT_SHAPE_REPRESENTATION(#107,#9698);
#167=CONTEXT_DEPENDENT_SHAPE_REPRESENTATION(#108,#9699);
#168=CONTEXT_DEPENDENT_SHAPE_REPRESENTATION(#109,#9700);
#169=CONTEXT_DEPENDENT_SHAPE_REPRESENTATION(#110,#9701);
#170=CONTEXT_DEPENDENT_SHAPE_REPRESENTATION(#111,#9702);
#171=CONTEXT_DEPENDENT_SHAPE_REPRESENTATION(#112,#9703);
#172=CONTEXT_DEPENDENT_SHAPE_REPRESENTATION(#113,#9704);
#173=CONTEXT_DEPENDENT_SHAPE_REPRESENTATION(#114,#9705);
#174=CONTEXT_DEPENDENT_SHAPE_REPRESENTATION(#115,#9706);
#175=CONTEXT_DEPENDENT_SHAPE_REPRESENTATION(#116,#9707);
#176=CONTEXT_DEPENDENT_SHAPE_REPRESENTATION(#117,#9708);
#177=CONTEXT_DEPENDENT_SHAPE_REPRESENTATION(#118,#9709);
#178=CONTEXT_DEPENDENT_SHAPE_REPRESENTATION(#119,#9710);
#179=CONTEXT_DEPENDENT_SHAPE_REPRESENTATION(#120,#9711);
#180=CONTEXT_DEPENDENT_SHAPE_REPRESENTATION(#121,#9712);
#181=CONTEXT_DEPENDENT_SHAPE_REPRESENTATION(#122,#9713);
#182=CONTEXT_DEPENDENT_SHAPE_REPRESENTATION(#123,#9714);
#183=CONTEXT_DEPENDENT_SHAPE_REPRESENTATION(#124,#9715);
#184=CONTEXT_DEPENDENT_SHAPE_REPRESENTATION(#125,#9716);
#185=CONTEXT_DEPENDENT_SHAPE_REPRESENTATION(#126,#9717);
#186=CONTEXT_DEPENDENT_SHAPE_REPRESENTATION(#127,#9718);
#187=CONTEXT_DEPENDENT_SHAPE_REPRESENTATION(#128,#9719);
#188=CONTEXT_DEPENDENT_SHAPE_REPRESENTATION(#129,#9720);
#189=CONTEXT_DEPENDENT_SHAPE_REPRESENTATION(#130,#9721);
#190=CONTEXT_DEPENDENT_SHAPE_REPRESENTATION(#131,#9722);
#191=CONTEXT_DEPENDENT_SHAPE_REPRESENTATION(#132,#9723);
#192=CONTEXT_DEPENDENT_SHAPE_REPRESENTATION(#133,#9724);
#193=CONTEXT_DEPENDENT_SHAPE_REPRESENTATION(#134,#9725);
#194=CONTEXT_DEPENDENT_SHAPE_REPRESENTATION(#135,#9726);
#195=CONTEXT_DEPENDENT_SHAPE_REPRESENTATION(#136,#9727);
#196=CONTEXT_DEPENDENT_SHAPE_REPRESENTATION(#137,#9728);
#197=CONTEXT_DEPENDENT_SHAPE_REPRESENTATION(#138,#9729);
#198=CONTEXT_DEPENDENT_SHAPE_REPRESENTATION(#139,#9730);
#199=CONTEXT_DEPENDENT_SHAPE_REPRESENTATION(#140,#9731);
#200=CONTEXT_DEPENDENT_SHAPE_REPRESENTATION(#141,#9732);
#201=CONTEXT_DEPENDENT_SHAPE_REPRESENTATION(#142,#9733);
#202=CONTEXT_DEPENDENT_SHAPE_REPRESENTATION(#143,#9734);
#203=CONTEXT_DEPENDENT_SHAPE_REPRESENTATION(#144,#9735);
#204=CONTEXT_DEPENDENT_SHAPE_REPRESENTATION(#145,#9736);
#205=CONTEXT_DEPENDENT_SHAPE_REPRESENTATION(#146,#9737);
#206=CONTEXT_DEPENDENT_SHAPE_REPRESENTATION(#147,#9738);
#207=CONTEXT_DEPENDENT_SHAPE_REPRESENTATION(#148,#9739);
#208=CONTEXT_DEPENDENT_SHAPE_REPRESENTATION(#149,#9740);
#209=CONTEXT_DEPENDENT_SHAPE_REPRESENTATION(#150,#9741);
#210=CONTEXT_DEPENDENT_SHAPE_REPRESENTATION(#151,#9742);
#211=CONTEXT_DEPENDENT_SHAPE_REPRESENTATION(#152,#9743);
#212=NEXT_ASSEMBLY_USAGE_OCCURRENCE('Inner ring:1','Inner ring:1',
'Inner ring:1',#9781,#9782,'Inner ring:1');
#213=NEXT_ASSEMBLY_USAGE_OCCURRENCE('Outer ring:1','Outer ring:1',
'Outer ring:1',#9781,#9783,'Outer ring:1');
#214=NEXT_ASSEMBLY_USAGE_OCCURRENCE('Balls:1','Balls:1','Balls:1',#9781,
#9784,'Balls:1');
#215=NEXT_ASSEMBLY_USAGE_OCCURRENCE('Cage:1','Cage:1','Cage:1',#9781,#9785,
'Cage:1');
#216=NEXT_ASSEMBLY_USAGE_OCCURRENCE('Seals 2RS:1','Seals 2RS:1',
'Seals 2RS:1',#9781,#9786,'Seals 2RS:1');
#217=NEXT_ASSEMBLY_USAGE_OCCURRENCE('Stepped axle:1','Stepped axle:1',
'Stepped axle:1',#9775,#9776,'Stepped axle:1');
#218=NEXT_ASSEMBLY_USAGE_OCCURRENCE('Journal spacer:1',
'Journal spacer:1','Journal spacer:1',#9775,#9777,'Journal spacer:1');
#219=NEXT_ASSEMBLY_USAGE_OCCURRENCE('Journal spacer (1):1',
'Journal spacer (1):1','Journal spacer (1):1',#9775,#9778,
'Journal spacer (1):1');
#220=NEXT_ASSEMBLY_USAGE_OCCURRENCE('End keeper:2','End keeper:2',
'End keeper:2',#9775,#9779,'End keeper:2');
#221=NEXT_ASSEMBLY_USAGE_OCCURRENCE('End keeper:3','End keeper:3',
'End keeper:3',#9775,#9779,'End keeper:3');
#222=NEXT_ASSEMBLY_USAGE_OCCURRENCE('Cap Screw - M4x16:2',
'Cap Screw - M4x16:2','Cap Screw - M4x16:2',#9775,#9802,
'Cap Screw - M4x16:2');
#223=NEXT_ASSEMBLY_USAGE_OCCURRENCE('Cap Screw - M4x16:3',
'Cap Screw - M4x16:3','Cap Screw - M4x16:3',#9775,#9802,
'Cap Screw - M4x16:3');
#224=NEXT_ASSEMBLY_USAGE_OCCURRENCE('Bracket shim:2','Bracket shim:2',
'Bracket shim:2',#9775,#9780,'Bracket shim:2');
#225=NEXT_ASSEMBLY_USAGE_OCCURRENCE('Bracket shim:3','Bracket shim:3',
'Bracket shim:3',#9775,#9780,'Bracket shim:3');
#226=NEXT_ASSEMBLY_USAGE_OCCURRENCE('Cleared radial bearing:2',
'Cleared radial bearing:2','Cleared radial bearing:2',#9775,#9781,
'Cleared radial bearing:2');
#227=NEXT_ASSEMBLY_USAGE_OCCURRENCE('Cleared radial bearing:3',
'Cleared radial bearing:3','Cleared radial bearing:3',#9775,#9781,
'Cleared radial bearing:3');
#228=NEXT_ASSEMBLY_USAGE_OCCURRENCE('Sliding axle block:1',
'Sliding axle block:1','Sliding axle block:1',#9775,#9787,
'Sliding axle block:1');
#229=NEXT_ASSEMBLY_USAGE_OCCURRENCE('Take-up screw bracket:1',
'Take-up screw bracket:1','Take-up screw bracket:1',#9775,#9788,
'Take-up screw bracket:1');
#230=NEXT_ASSEMBLY_USAGE_OCCURRENCE('Sliding axle block (1):1',
'Sliding axle block (1):1','Sliding axle block (1):1',#9775,#9789,
'Sliding axle block (1):1');
#231=NEXT_ASSEMBLY_USAGE_OCCURRENCE('Take-up screw bracket (1):1',
'Take-up screw bracket (1):1','Take-up screw bracket (1):1',#9775,#9790,
'Take-up screw bracket (1):1');
#232=NEXT_ASSEMBLY_USAGE_OCCURRENCE(
'Slotted Extrusion - 20 x 20 x 100 mm:2',
'Slotted Extrusion - 20 x 20 x 100 mm:2',
'Slotted Extrusion - 20 x 20 x 100 mm:2',#9775,#9791,
'Slotted Extrusion - 20 x 20 x 100 mm:2');
#233=NEXT_ASSEMBLY_USAGE_OCCURRENCE(
'Slot Nut - M5 for 20 mm Extrusion:2',
'Slot Nut - M5 for 20 mm Extrusion:2',
'Slot Nut - M5 for 20 mm Extrusion:2',#9775,#9792,
'Slot Nut - M5 for 20 mm Extrusion:2');
#234=NEXT_ASSEMBLY_USAGE_OCCURRENCE('Flat Washer - M5:2',
'Flat Washer - M5:2','Flat Washer - M5:2',#9775,#9793,
'Flat Washer - M5:2');
#235=NEXT_ASSEMBLY_USAGE_OCCURRENCE('M5x14 Cap Screw:2',
'M5x14 Cap Screw:2','M5x14 Cap Screw:2',#9775,#9794,'M5x14 Cap Screw:2');
#236=NEXT_ASSEMBLY_USAGE_OCCURRENCE(
'Slot Nut - M5 for 20 mm Extrusion:3',
'Slot Nut - M5 for 20 mm Extrusion:3',
'Slot Nut - M5 for 20 mm Extrusion:3',#9775,#9792,
'Slot Nut - M5 for 20 mm Extrusion:3');
#237=NEXT_ASSEMBLY_USAGE_OCCURRENCE('Flat Washer - M5:3',
'Flat Washer - M5:3','Flat Washer - M5:3',#9775,#9793,
'Flat Washer - M5:3');
#238=NEXT_ASSEMBLY_USAGE_OCCURRENCE('M5x14 Cap Screw:3',
'M5x14 Cap Screw:3','M5x14 Cap Screw:3',#9775,#9794,'M5x14 Cap Screw:3');
#239=NEXT_ASSEMBLY_USAGE_OCCURRENCE(
'Slot Nut - M5 for 20 mm Extrusion:4',
'Slot Nut - M5 for 20 mm Extrusion:4',
'Slot Nut - M5 for 20 mm Extrusion:4',#9775,#9792,
'Slot Nut - M5 for 20 mm Extrusion:4');
#240=NEXT_ASSEMBLY_USAGE_OCCURRENCE('Flat Washer - M5:4',
'Flat Washer - M5:4','Flat Washer - M5:4',#9775,#9793,
'Flat Washer - M5:4');
#241=NEXT_ASSEMBLY_USAGE_OCCURRENCE('M5x14 Cap Screw:4',
'M5x14 Cap Screw:4','M5x14 Cap Screw:4',#9775,#9794,'M5x14 Cap Screw:4');
#242=NEXT_ASSEMBLY_USAGE_OCCURRENCE('Hex Bolt - M8x40:2',
'Hex Bolt - M8x40:2','Hex Bolt - M8x40:2',#9775,#9795,
'Hex Bolt - M8x40:2');
#243=NEXT_ASSEMBLY_USAGE_OCCURRENCE('Hex Nut - M8:2','Hex Nut - M8:2',
'Hex Nut - M8:2',#9775,#9796,'Hex Nut - M8:2');
#244=NEXT_ASSEMBLY_USAGE_OCCURRENCE(
'Slotted Extrusion - 20 x 20 x 100 mm:3',
'Slotted Extrusion - 20 x 20 x 100 mm:3',
'Slotted Extrusion - 20 x 20 x 100 mm:3',#9775,#9791,
'Slotted Extrusion - 20 x 20 x 100 mm:3');
#245=NEXT_ASSEMBLY_USAGE_OCCURRENCE(
'Slot Nut - M5 for 20 mm Extrusion:5',
'Slot Nut - M5 for 20 mm Extrusion:5',
'Slot Nut - M5 for 20 mm Extrusion:5',#9775,#9792,
'Slot Nut - M5 for 20 mm Extrusion:5');
#246=NEXT_ASSEMBLY_USAGE_OCCURRENCE('Flat Washer - M5:5',
'Flat Washer - M5:5','Flat Washer - M5:5',#9775,#9793,
'Flat Washer - M5:5');
#247=NEXT_ASSEMBLY_USAGE_OCCURRENCE('M5x14 Cap Screw:5',
'M5x14 Cap Screw:5','M5x14 Cap Screw:5',#9775,#9794,'M5x14 Cap Screw:5');
#248=NEXT_ASSEMBLY_USAGE_OCCURRENCE(
'Slot Nut - M5 for 20 mm Extrusion:6',
'Slot Nut - M5 for 20 mm Extrusion:6',
'Slot Nut - M5 for 20 mm Extrusion:6',#9775,#9792,
'Slot Nut - M5 for 20 mm Extrusion:6');
#249=NEXT_ASSEMBLY_USAGE_OCCURRENCE('Flat Washer - M5:6',
'Flat Washer - M5:6','Flat Washer - M5:6',#9775,#9793,
'Flat Washer - M5:6');
#250=NEXT_ASSEMBLY_USAGE_OCCURRENCE('M5x14 Cap Screw:6',
'M5x14 Cap Screw:6','M5x14 Cap Screw:6',#9775,#9794,'M5x14 Cap Screw:6');
#251=NEXT_ASSEMBLY_USAGE_OCCURRENCE(
'Slot Nut - M5 for 20 mm Extrusion:7',
'Slot Nut - M5 for 20 mm Extrusion:7',
'Slot Nut - M5 for 20 mm Extrusion:7',#9775,#9792,
'Slot Nut - M5 for 20 mm Extrusion:7');
#252=NEXT_ASSEMBLY_USAGE_OCCURRENCE('Flat Washer - M5:7',
'Flat Washer - M5:7','Flat Washer - M5:7',#9775,#9793,
'Flat Washer - M5:7');
#253=NEXT_ASSEMBLY_USAGE_OCCURRENCE('M5x14 Cap Screw:7',
'M5x14 Cap Screw:7','M5x14 Cap Screw:7',#9775,#9794,'M5x14 Cap Screw:7');
#254=NEXT_ASSEMBLY_USAGE_OCCURRENCE('Hex Bolt - M8x40:3',
'Hex Bolt - M8x40:3','Hex Bolt - M8x40:3',#9775,#9795,
'Hex Bolt - M8x40:3');
#255=NEXT_ASSEMBLY_USAGE_OCCURRENCE('Hex Nut - M8:3','Hex Nut - M8:3',
'Hex Nut - M8:3',#9775,#9796,'Hex Nut - M8:3');
#256=NEXT_ASSEMBLY_USAGE_OCCURRENCE('Bearing insert:1',
'Bearing insert:1','Bearing insert:1',#9797,#9798,'Bearing insert:1');
#257=NEXT_ASSEMBLY_USAGE_OCCURRENCE('Bearing insert (1):1',
'Bearing insert (1):1','Bearing insert (1):1',#9797,#9799,
'Bearing insert (1):1');
#258=NEXT_ASSEMBLY_USAGE_OCCURRENCE('Roller tube:2','Roller tube:2',
'Roller tube:2',#9797,#9800,'Roller tube:2');
#259=NEXT_ASSEMBLY_USAGE_OCCURRENCE('Outer race retainer:2',
'Outer race retainer:2','Outer race retainer:2',#9797,#9801,
'Outer race retainer:2');
#260=NEXT_ASSEMBLY_USAGE_OCCURRENCE('Cap Screw - M4x16:4',
'Cap Screw - M4x16:4','Cap Screw - M4x16:4',#9797,#9802,
'Cap Screw - M4x16:4');
#261=NEXT_ASSEMBLY_USAGE_OCCURRENCE('Cap Screw - M4x16:5',
'Cap Screw - M4x16:5','Cap Screw - M4x16:5',#9797,#9802,
'Cap Screw - M4x16:5');
#262=NEXT_ASSEMBLY_USAGE_OCCURRENCE('Cap Screw - M4x16:6',
'Cap Screw - M4x16:6','Cap Screw - M4x16:6',#9797,#9802,
'Cap Screw - M4x16:6');
#263=NEXT_ASSEMBLY_USAGE_OCCURRENCE('Cap Screw - M4x16:7',
'Cap Screw - M4x16:7','Cap Screw - M4x16:7',#9797,#9802,
'Cap Screw - M4x16:7');
#264=NEXT_ASSEMBLY_USAGE_OCCURRENCE('Outer race retainer:3',
'Outer race retainer:3','Outer race retainer:3',#9797,#9801,
'Outer race retainer:3');
#265=NEXT_ASSEMBLY_USAGE_OCCURRENCE('Cap Screw - M4x16:8',
'Cap Screw - M4x16:8','Cap Screw - M4x16:8',#9797,#9802,
'Cap Screw - M4x16:8');
#266=NEXT_ASSEMBLY_USAGE_OCCURRENCE('Cap Screw - M4x16:9',
'Cap Screw - M4x16:9','Cap Screw - M4x16:9',#9797,#9802,
'Cap Screw - M4x16:9');
#267=NEXT_ASSEMBLY_USAGE_OCCURRENCE('Cap Screw - M4x16:10',
'Cap Screw - M4x16:10','Cap Screw - M4x16:10',#9797,#9802,
'Cap Screw - M4x16:10');
#268=NEXT_ASSEMBLY_USAGE_OCCURRENCE('Cap Screw - M4x16:11',
'Cap Screw - M4x16:11','Cap Screw - M4x16:11',#9797,#9802,
'Cap Screw - M4x16:11');
#269=NEXT_ASSEMBLY_USAGE_OCCURRENCE('Axle brackets and bearings:1',
'Axle brackets and bearings:1','Axle brackets and bearings:1',#9774,#9775,
'Axle brackets and bearings:1');
#270=NEXT_ASSEMBLY_USAGE_OCCURRENCE('Roller tube and end caps:1',
'Roller tube and end caps:1','Roller tube and end caps:1',#9774,#9797,
'Roller tube and end caps:1');
#271=B_SPLINE_CURVE_WITH_KNOTS('',3,(#7915,#7916,#7917,#7918,#7919,#7920,
#7921,#7922,#7923,#7924,#7925,#7926,#7927,#7928,#7929,#7930,#7931,#7932,
#7933,#7934,#7935,#7936),.UNSPECIFIED.,.F.,.F.,(4,2,2,2,2,2,2,2,2,2,4),
(0.0473477652366656,0.126350602536658,0.189525903804987,0.252701205073317,
0.313298422430275,0.373895639787233,0.434492857144191,0.495090074501149,
0.558265375769478,0.621440677037807,0.7004435143378),.UNSPECIFIED.);
#272=B_SPLINE_CURVE_WITH_KNOTS('',3,(#7940,#7941,#7942,#7943,#7944,#7945,
#7946,#7947,#7948,#7949,#7950,#7951,#7952,#7953,#7954,#7955,#7956,#7957,
#7958,#7959,#7960,#7961),.UNSPECIFIED.,.F.,.F.,(4,2,2,2,2,2,2,2,2,2,4),
(0.0464897534940957,0.0852567806515119,0.170513561303024,0.246687263103517,
0.308657850341199,0.370628437578881,0.432599024816563,0.494569612054245,
0.570743313854739,0.656000094506251,0.694767121663666),.UNSPECIFIED.);
#273=B_SPLINE_CURVE_WITH_KNOTS('',3,(#7967,#7968,#7969,#7970,#7971,#7972,
#7973,#7974,#7975,#7976,#7977,#7978,#7979,#7980,#7981,#7982,#7983,#7984,
#7985,#7986,#7987,#7988),.UNSPECIFIED.,.F.,.F.,(4,2,2,2,2,2,2,2,2,2,4),
(0.0464897534940957,0.0852567806515118,0.170513561303024,0.246687263103517,
0.308657850341199,0.370628437578881,0.432599024816563,0.494569612054245,
0.570743313854738,0.65600009450625,0.694767121663666),.UNSPECIFIED.);
#274=B_SPLINE_CURVE_WITH_KNOTS('',3,(#7992,#7993,#7994,#7995,#7996,#7997,
#7998,#7999,#8000,#8001,#8002,#8003,#8004,#8005,#8006,#8007,#8008,#8009,
#8010,#8011,#8012,#8013),.UNSPECIFIED.,.F.,.F.,(4,2,2,2,2,2,2,2,2,2,4),
(0.0464897534940957,0.0852567806515119,0.170513561303024,0.246687263103517,
0.308657850341199,0.370628437578881,0.432599024816563,0.494569612054245,
0.570743313854739,0.656000094506251,0.694767121663666),.UNSPECIFIED.);
#275=B_SPLINE_CURVE_WITH_KNOTS('',3,(#8017,#8018,#8019,#8020,#8021,#8022,
#8023,#8024,#8025,#8026,#8027,#8028),.UNSPECIFIED.,.F.,.F.,(4,2,2,2,2,4),
(0.0464897534940957,0.0852567806515119,0.170513561303024,0.246687263103517,
0.308657850341199,0.370628437578881),.UNSPECIFIED.);
#276=B_SPLINE_CURVE_WITH_KNOTS('',3,(#8033,#8034,#8035,#8036,#8037,#8038,
#8039,#8040,#8041,#8042,#8043,#8044),.UNSPECIFIED.,.F.,.F.,(4,2,2,2,2,4),
(0.370628437578881,0.432599024816563,0.494569612054245,0.570743313854738,
0.65600009450625,0.694767121663666),.UNSPECIFIED.);
#277=B_SPLINE_CURVE_WITH_KNOTS('',3,(#8048,#8049,#8050,#8051,#8052,#8053,
#8054,#8055,#8056,#8057,#8058,#8059,#8060,#8061,#8062,#8063,#8064,#8065,
#8066,#8067,#8068,#8069),.UNSPECIFIED.,.F.,.F.,(4,2,2,2,2,2,2,2,2,2,4),
(0.0464897534940957,0.0852567806515121,0.170513561303024,0.246687263103518,
0.308657850341199,0.370628437578881,0.432599024816563,0.494569612054245,
0.570743313854738,0.65600009450625,0.694767121663666),.UNSPECIFIED.);
#278=B_SPLINE_CURVE_WITH_KNOTS('',3,(#8073,#8074,#8075,#8076,#8077,#8078,
#8079,#8080,#8081,#8082,#8083,#8084,#8085,#8086,#8087,#8088,#8089,#8090,
#8091,#8092,#8093,#8094),.UNSPECIFIED.,.F.,.F.,(4,2,2,2,2,2,2,2,2,2,4),
(0.0464897534940957,0.0852567806515119,0.170513561303024,0.246687263103517,
0.308657850341199,0.370628437578881,0.432599024816563,0.494569612054245,
0.570743313854738,0.65600009450625,0.694767121663667),.UNSPECIFIED.);
#279=B_SPLINE_CURVE_WITH_KNOTS('',3,(#8098,#8099,#8100,#8101,#8102,#8103,
#8104,#8105,#8106,#8107,#8108,#8109,#8110,#8111,#8112,#8113,#8114,#8115,
#8116,#8117,#8118,#8119),.UNSPECIFIED.,.F.,.F.,(4,2,2,2,2,2,2,2,2,2,4),
(0.0464897534940957,0.0852567806515119,0.170513561303024,0.246687263103517,
0.308657850341199,0.370628437578881,0.432599024816563,0.494569612054245,
0.570743313854738,0.65600009450625,0.694767121663666),.UNSPECIFIED.);
#280=B_SPLINE_CURVE_WITH_KNOTS('',3,(#8123,#8124,#8125,#8126,#8127,#8128,
#8129,#8130,#8131,#8132,#8133,#8134,#8135,#8136,#8137,#8138,#8139,#8140,
#8141,#8142,#8143,#8144),.UNSPECIFIED.,.F.,.F.,(4,2,2,2,2,2,2,2,2,2,4),
(0.0464897534940957,0.0852567806515119,0.170513561303024,0.246687263103517,
0.308657850341199,0.370628437578881,0.432599024816563,0.494569612054245,
0.570743313854739,0.656000094506251,0.694767121663667),.UNSPECIFIED.);
#281=B_SPLINE_CURVE_WITH_KNOTS('',3,(#8152,#8153,#8154,#8155,#8156,#8157,
#8158,#8159,#8160,#8161,#8162,#8163,#8164,#8165,#8166,#8167,#8168,#8169,
#8170,#8171,#8172,#8173),.UNSPECIFIED.,.F.,.F.,(4,2,2,2,2,2,2,2,2,2,4),
(0.0473477652366656,0.126350602536658,0.189525903804987,0.252701205073316,
0.313298422430274,0.373895639787232,0.434492857144191,0.495090074501149,
0.558265375769478,0.621440677037807,0.7004435143378),.UNSPECIFIED.);
#282=B_SPLINE_CURVE_WITH_KNOTS('',3,(#8181,#8182,#8183,#8184,#8185,#8186,
#8187,#8188,#8189,#8190,#8191,#8192,#8193,#8194,#8195,#8196,#8197,#8198,
#8199,#8200,#8201,#8202),.UNSPECIFIED.,.F.,.F.,(4,2,2,2,2,2,2,2,2,2,4),
(0.0473477652366656,0.126350602536658,0.189525903804987,0.252701205073317,
0.313298422430275,0.373895639787233,0.434492857144191,0.495090074501149,
0.558265375769478,0.621440677037807,0.7004435143378),.UNSPECIFIED.);
#283=B_SPLINE_CURVE_WITH_KNOTS('',3,(#8211,#8212,#8213,#8214,#8215,#8216,
#8217,#8218,#8219,#8220,#8221,#8222),.UNSPECIFIED.,.F.,.F.,(4,2,2,2,2,4),
(0.0473477652366656,0.126350602536658,0.189525903804987,0.252701205073316,
0.313298422430275,0.373895639787233),.UNSPECIFIED.);
#284=B_SPLINE_CURVE_WITH_KNOTS('',3,(#8224,#8225,#8226,#8227,#8228,#8229,
#8230,#8231,#8232,#8233,#8234,#8235),.UNSPECIFIED.,.F.,.F.,(4,2,2,2,2,4),
(0.373895639787233,0.434492857144191,0.495090074501149,0.558265375769478,
0.621440677037807,0.7004435143378),.UNSPECIFIED.);
#285=B_SPLINE_CURVE_WITH_KNOTS('',3,(#8242,#8243,#8244,#8245,#8246,#8247,
#8248,#8249,#8250,#8251,#8252,#8253,#8254,#8255,#8256,#8257,#8258,#8259,
#8260,#8261,#8262,#8263),.UNSPECIFIED.,.F.,.F.,(4,2,2,2,2,2,2,2,2,2,4),
(0.0473477652366656,0.126350602536658,0.189525903804987,0.252701205073316,
0.313298422430275,0.373895639787233,0.434492857144191,0.495090074501149,
0.558265375769478,0.621440677037807,0.7004435143378),.UNSPECIFIED.);
#286=B_SPLINE_CURVE_WITH_KNOTS('',3,(#8271,#8272,#8273,#8274,#8275,#8276,
#8277,#8278,#8279,#8280,#8281,#8282,#8283,#8284,#8285,#8286,#8287,#8288,
#8289,#8290,#8291,#8292),.UNSPECIFIED.,.F.,.F.,(4,2,2,2,2,2,2,2,2,2,4),
(0.0473477652366656,0.126350602536658,0.189525903804987,0.252701205073317,
0.313298422430275,0.373895639787233,0.434492857144191,0.495090074501149,
0.558265375769478,0.621440677037807,0.7004435143378),.UNSPECIFIED.);
#287=B_SPLINE_CURVE_WITH_KNOTS('',3,(#8300,#8301,#8302,#8303,#8304,#8305,
#8306,#8307,#8308,#8309,#8310,#8311,#8312,#8313,#8314,#8315,#8316,#8317,
#8318,#8319,#8320,#8321),.UNSPECIFIED.,.F.,.F.,(4,2,2,2,2,2,2,2,2,2,4),
(0.0473477652366656,0.126350602536658,0.189525903804987,0.252701205073316,
0.313298422430275,0.373895639787233,0.434492857144191,0.495090074501149,
0.558265375769478,0.621440677037807,0.7004435143378),.UNSPECIFIED.);
#288=B_SPLINE_CURVE_WITH_KNOTS('',3,(#8330,#8331,#8332,#8333,#8334,#8335,
#8336,#8337,#8338,#8339,#8340,#8341,#8342,#8343,#8344,#8345,#8346,#8347,
#8348,#8349,#8350,#8351),.UNSPECIFIED.,.F.,.F.,(4,2,2,2,2,2,2,2,2,2,4),
(0.0473477652366656,0.126350602536658,0.189525903804987,0.252701205073317,
0.313298422430275,0.373895639787233,0.434492857144191,0.495090074501149,
0.558265375769478,0.621440677037807,0.7004435143378),.UNSPECIFIED.);
#289=SPHERICAL_SURFACE('',#5611,0.23815);
#290=SPHERICAL_SURFACE('',#5613,0.23815);
#291=SPHERICAL_SURFACE('',#5615,0.23815);
#292=SPHERICAL_SURFACE('',#5617,0.23815);
#293=SPHERICAL_SURFACE('',#5619,0.23815);
#294=SPHERICAL_SURFACE('',#5621,0.23815);
#295=SPHERICAL_SURFACE('',#5623,0.23815);
#296=SPHERICAL_SURFACE('',#5625,0.23815);
#297=SPHERICAL_SURFACE('',#5628,0.247676);
#298=SPHERICAL_SURFACE('',#5644,0.247676);
#299=SPHERICAL_SURFACE('',#5649,0.247676);
#300=SPHERICAL_SURFACE('',#5654,0.247676);
#301=SPHERICAL_SURFACE('',#5659,0.247676);
#302=SPHERICAL_SURFACE('',#5664,0.247676);
#303=SPHERICAL_SURFACE('',#5669,0.247676);
#304=SPHERICAL_SURFACE('',#5677,0.247676);
#305=CONICAL_SURFACE('',#5582,0.53,0.785398163397448);
#306=CONICAL_SURFACE('',#5589,0.53,0.785398163397448);
#307=CONICAL_SURFACE('',#5602,1.47,0.785398163397449);
#308=CONICAL_SURFACE('',#5606,1.47,0.785398163397449);
#309=CONICAL_SURFACE('',#5879,0.275,0.785398163397449);
#310=CONICAL_SURFACE('',#5902,0.4,0.785398163397448);
#311=CONICAL_SURFACE('',#5906,0.41,0.785398163397448);
#312=CONICAL_SURFACE('',#5910,0.26,0.463647609000806);
#313=CONICAL_SURFACE('',#5917,0.36,0.785398163397451);
#314=CONICAL_SURFACE('',#5920,0.734027674973257,1.0471975511966);
#315=CONICAL_SURFACE('',#5931,0.734027674973257,1.0471975511966);
#316=CONICAL_SURFACE('',#5933,0.734027674973257,1.0471975511966);
#317=CONICAL_SURFACE('',#6030,0.325,0.785398163397448);
#318=CONICAL_SURFACE('',#6034,0.335,0.785398163397448);
#319=CONICAL_SURFACE('',#6038,0.21,0.463647609000806);
#320=CONICAL_SURFACE('',#6042,0.18,0.785398163397448);
#321=TOROIDAL_SURFACE('',#5571,1.,0.247676);
#322=TOROIDAL_SURFACE('',#5591,1.,0.247676);
#323=SHAPE_REPRESENTATION_RELATIONSHIP('SRR','None',#9746,#348);
#324=SHAPE_REPRESENTATION_RELATIONSHIP('SRR','None',#9747,#349);
#325=SHAPE_REPRESENTATION_RELATIONSHIP('SRR','None',#9748,#350);
#326=SHAPE_REPRESENTATION_RELATIONSHIP('SRR','None',#9749,#351);
#327=SHAPE_REPRESENTATION_RELATIONSHIP('SRR','None',#9750,#352);
#328=SHAPE_REPRESENTATION_RELATIONSHIP('SRR','None',#9752,#353);
#329=SHAPE_REPRESENTATION_RELATIONSHIP('SRR','None',#9753,#354);
#330=SHAPE_REPRESENTATION_RELATIONSHIP('SRR','None',#9754,#355);
#331=SHAPE_REPRESENTATION_RELATIONSHIP('SRR','None',#9755,#356);
#332=SHAPE_REPRESENTATION_RELATIONSHIP('SRR','None',#9756,#357);
#333=SHAPE_REPRESENTATION_RELATIONSHIP('SRR','None',#9757,#358);
#334=SHAPE_REPRESENTATION_RELATIONSHIP('SRR','None',#9758,#359);
#335=SHAPE_REPRESENTATION_RELATIONSHIP('SRR','None',#9759,#360);
#336=SHAPE_REPRESENTATION_RELATIONSHIP('SRR','None',#9760,#361);
#337=SHAPE_REPRESENTATION_RELATIONSHIP('SRR','None',#9761,#362);
#338=SHAPE_REPRESENTATION_RELATIONSHIP('SRR','None',#9762,#363);
#339=SHAPE_REPRESENTATION_RELATIONSHIP('SRR','None',#9763,#364);
#340=SHAPE_REPRESENTATION_RELATIONSHIP('SRR','None',#9764,#365);
#341=SHAPE_REPRESENTATION_RELATIONSHIP('SRR','None',#9765,#366);
#342=SHAPE_REPRESENTATION_RELATIONSHIP('SRR','None',#9766,#367);
#343=SHAPE_REPRESENTATION_RELATIONSHIP('SRR','None',#9768,#368);
#344=SHAPE_REPRESENTATION_RELATIONSHIP('SRR','None',#9769,#369);
#345=SHAPE_REPRESENTATION_RELATIONSHIP('SRR','None',#9770,#370);
#346=SHAPE_REPRESENTATION_RELATIONSHIP('SRR','None',#9771,#371);
#347=SHAPE_REPRESENTATION_RELATIONSHIP('SRR','None',#9772,#372);
#348=ADVANCED_BREP_SHAPE_REPRESENTATION('',(#406),#9595);
#349=ADVANCED_BREP_SHAPE_REPRESENTATION('',(#407),#9596);
#350=ADVANCED_BREP_SHAPE_REPRESENTATION('',(#408),#9597);
#351=ADVANCED_BREP_SHAPE_REPRESENTATION('',(#409),#9598);
#352=ADVANCED_BREP_SHAPE_REPRESENTATION('',(#410),#9599);
#353=ADVANCED_BREP_SHAPE_REPRESENTATION('',(#411),#9601);
#354=ADVANCED_BREP_SHAPE_REPRESENTATION('',(#412),#9602);
#355=ADVANCED_BREP_SHAPE_REPRESENTATION('',(#413,#414,#415,#416,#417,#418,
#419,#420),#9603);
#356=ADVANCED_BREP_SHAPE_REPRESENTATION('',(#421),#9604);
#357=ADVANCED_BREP_SHAPE_REPRESENTATION('',(#422,#423),#9605);
#358=ADVANCED_BREP_SHAPE_REPRESENTATION('',(#424),#9606);
#359=ADVANCED_BREP_SHAPE_REPRESENTATION('',(#425),#9607);
#360=ADVANCED_BREP_SHAPE_REPRESENTATION('',(#426),#9608);
#361=ADVANCED_BREP_SHAPE_REPRESENTATION('',(#427),#9609);
#362=ADVANCED_BREP_SHAPE_REPRESENTATION('',(#428),#9610);
#363=ADVANCED_BREP_SHAPE_REPRESENTATION('',(#429),#9611);
#364=ADVANCED_BREP_SHAPE_REPRESENTATION('',(#430),#9612);
#365=ADVANCED_BREP_SHAPE_REPRESENTATION('',(#31),#9613);
#366=ADVANCED_BREP_SHAPE_REPRESENTATION('',(#431),#9614);
#367=ADVANCED_BREP_SHAPE_REPRESENTATION('',(#432),#9615);
#368=ADVANCED_BREP_SHAPE_REPRESENTATION('',(#433),#9617);
#369=ADVANCED_BREP_SHAPE_REPRESENTATION('',(#434),#9618);
#370=ADVANCED_BREP_SHAPE_REPRESENTATION('',(#435),#9619);
#371=ADVANCED_BREP_SHAPE_REPRESENTATION('',(#436),#9620);
#372=ADVANCED_BREP_SHAPE_REPRESENTATION('',(#32),#9621);
#373=STYLED_ITEM('',(#9962),#406);
#374=STYLED_ITEM('',(#9955),#407);
#375=STYLED_ITEM('',(#9955),#408);
#376=STYLED_ITEM('',(#9976),#409);
#377=STYLED_ITEM('',(#9941),#410);
#378=STYLED_ITEM('',(#9962),#411);
#379=STYLED_ITEM('',(#9962),#412);
#380=STYLED_ITEM('',(#9962),#413);
#381=STYLED_ITEM('',(#9962),#414);
#382=STYLED_ITEM('',(#9962),#415);
#383=STYLED_ITEM('',(#9962),#416);
#384=STYLED_ITEM('',(#9962),#417);
#385=STYLED_ITEM('',(#9962),#418);
#386=STYLED_ITEM('',(#9962),#419);
#387=STYLED_ITEM('',(#9962),#420);
#388=STYLED_ITEM('',(#9962),#421);
#389=STYLED_ITEM('',(#9962),#422);
#390=STYLED_ITEM('',(#9962),#423);
#391=STYLED_ITEM('',(#9962),#424);
#392=STYLED_ITEM('',(#9969),#425);
#393=STYLED_ITEM('',(#9962),#426);
#394=STYLED_ITEM('',(#9969),#427);
#395=STYLED_ITEM('',(#9976),#428);
#396=STYLED_ITEM('',(#9969),#429);
#397=STYLED_ITEM('',(#9969),#430);
#398=STYLED_ITEM('',(#9969),#31);
#399=STYLED_ITEM('',(#9969),#431);
#400=STYLED_ITEM('',(#9969),#432);
#401=STYLED_ITEM('',(#9962),#433);
#402=STYLED_ITEM('',(#9962),#434);
#403=STYLED_ITEM('',(#9948),#435);
#404=STYLED_ITEM('',(#9962),#436);
#405=STYLED_ITEM('',(#9969),#32);
#406=MANIFOLD_SOLID_BREP('Body1',#5198);
#407=MANIFOLD_SOLID_BREP('Body1',#5199);
#408=MANIFOLD_SOLID_BREP('Body1',#5200);
#409=MANIFOLD_SOLID_BREP('Body1',#5201);
#410=MANIFOLD_SOLID_BREP('Body1',#5202);
#411=MANIFOLD_SOLID_BREP('Body1',#5203);
#412=MANIFOLD_SOLID_BREP('Body1',#5204);
#413=MANIFOLD_SOLID_BREP('Body1',#5205);
#414=MANIFOLD_SOLID_BREP('Body2',#5206);
#415=MANIFOLD_SOLID_BREP('Body3',#5207);
#416=MANIFOLD_SOLID_BREP('Body4',#5208);
#417=MANIFOLD_SOLID_BREP('Body5',#5209);
#418=MANIFOLD_SOLID_BREP('Body6',#5210);
#419=MANIFOLD_SOLID_BREP('Body7',#5211);
#420=MANIFOLD_SOLID_BREP('Body8',#5212);
#421=MANIFOLD_SOLID_BREP('Continuous crown cage',#5213);
#422=MANIFOLD_SOLID_BREP('Body1',#5214);
#423=MANIFOLD_SOLID_BREP('Body2',#5215);
#424=MANIFOLD_SOLID_BREP('Body1',#5216);
#425=MANIFOLD_SOLID_BREP('Body1',#5217);
#426=MANIFOLD_SOLID_BREP('Body1',#5218);
#427=MANIFOLD_SOLID_BREP('Body1',#5219);
#428=MANIFOLD_SOLID_BREP('Body1',#5220);
#429=MANIFOLD_SOLID_BREP('Body1',#5221);
#430=MANIFOLD_SOLID_BREP('Body1',#5222);
#431=MANIFOLD_SOLID_BREP('Body1',#5225);
#432=MANIFOLD_SOLID_BREP('Body1',#5226);
#433=MANIFOLD_SOLID_BREP('Body1',#5227);
#434=MANIFOLD_SOLID_BREP('Body1',#5228);
#435=MANIFOLD_SOLID_BREP('Body1',#5229);
#436=MANIFOLD_SOLID_BREP('Body1',#5230);
#437=FACE_BOUND('',#1016,.T.);
#438=FACE_BOUND('',#1018,.T.);
#439=FACE_BOUND('',#1023,.T.);
#440=FACE_BOUND('',#1025,.T.);
#441=FACE_BOUND('',#1029,.T.);
#442=FACE_BOUND('',#1031,.T.);
#443=FACE_BOUND('',#1035,.T.);
#444=FACE_BOUND('',#1037,.T.);
#445=FACE_BOUND('',#1041,.T.);
#446=FACE_BOUND('',#1043,.T.);
#447=FACE_BOUND('',#1047,.T.);
#448=FACE_BOUND('',#1049,.T.);
#449=FACE_BOUND('',#1055,.T.);
#450=FACE_BOUND('',#1058,.T.);
#451=FACE_BOUND('',#1063,.T.);
#452=FACE_BOUND('',#1068,.T.);
#453=FACE_BOUND('',#1096,.T.);
#454=FACE_BOUND('',#1099,.T.);
#455=FACE_BOUND('',#1102,.T.);
#456=FACE_BOUND('',#1105,.T.);
#457=FACE_BOUND('',#1108,.T.);
#458=FACE_BOUND('',#1114,.T.);
#459=FACE_BOUND('',#1119,.T.);
#460=FACE_BOUND('',#1135,.T.);
#461=FACE_BOUND('',#1136,.T.);
#462=FACE_BOUND('',#1137,.T.);
#463=FACE_BOUND('',#1138,.T.);
#464=FACE_BOUND('',#1139,.T.);
#465=FACE_BOUND('',#1141,.T.);
#466=FACE_BOUND('',#1142,.T.);
#467=FACE_BOUND('',#1147,.T.);
#468=FACE_BOUND('',#1149,.T.);
#469=FACE_BOUND('',#1154,.T.);
#470=FACE_BOUND('',#1156,.T.);
#471=FACE_BOUND('',#1161,.T.);
#472=FACE_BOUND('',#1166,.T.);
#473=FACE_BOUND('',#1182,.T.);
#474=FACE_BOUND('',#1183,.T.);
#475=FACE_BOUND('',#1184,.T.);
#476=FACE_BOUND('',#1185,.T.);
#477=FACE_BOUND('',#1186,.T.);
#478=FACE_BOUND('',#1188,.T.);
#479=FACE_BOUND('',#1189,.T.);
#480=FACE_BOUND('',#1194,.T.);
#481=FACE_BOUND('',#1196,.T.);
#482=FACE_BOUND('',#1201,.T.);
#483=FACE_BOUND('',#1203,.T.);
#484=FACE_BOUND('',#1250,.T.);
#485=FACE_BOUND('',#1252,.T.);
#486=FACE_BOUND('',#1263,.T.);
#487=FACE_BOUND('',#1267,.T.);
#488=FACE_BOUND('',#1270,.T.);
#489=FACE_BOUND('',#1285,.T.);
#490=FACE_BOUND('',#1300,.T.);
#491=FACE_BOUND('',#1311,.T.);
#492=FACE_BOUND('',#1313,.T.);
#493=FACE_BOUND('',#1320,.T.);
#494=FACE_BOUND('',#1324,.T.);
#495=FACE_BOUND('',#1325,.T.);
#496=FACE_BOUND('',#1326,.T.);
#497=FACE_BOUND('',#1327,.T.);
#498=FACE_BOUND('',#1328,.T.);
#499=FACE_BOUND('',#1330,.T.);
#500=FACE_BOUND('',#1331,.T.);
#501=FACE_BOUND('',#1332,.T.);
#502=FACE_BOUND('',#1333,.T.);
#503=FACE_BOUND('',#1334,.T.);
#504=FACE_BOUND('',#1341,.T.);
#505=FACE_BOUND('',#1345,.T.);
#506=FACE_BOUND('',#1346,.T.);
#507=FACE_BOUND('',#1347,.T.);
#508=FACE_BOUND('',#1348,.T.);
#509=FACE_BOUND('',#1349,.T.);
#510=FACE_BOUND('',#1351,.T.);
#511=FACE_BOUND('',#1352,.T.);
#512=FACE_BOUND('',#1353,.T.);
#513=FACE_BOUND('',#1354,.T.);
#514=FACE_BOUND('',#1355,.T.);
#515=FACE_BOUND('',#1359,.T.);
#516=FACE_BOUND('',#1361,.T.);
#517=FACE_BOUND('',#1369,.T.);
#518=FACE_BOUND('',#1370,.T.);
#519=FACE_BOUND('',#1371,.T.);
#520=FACE_BOUND('',#1372,.T.);
#521=FACE_BOUND('',#1373,.T.);
#522=FACE_BOUND('',#1375,.T.);
#523=FACE_BOUND('',#1376,.T.);
#524=FACE_BOUND('',#1377,.T.);
#525=FACE_BOUND('',#1378,.T.);
#526=FACE_BOUND('',#1379,.T.);
#527=FACE_BOUND('',#1385,.T.);
#528=PLANE('',#5515);
#529=PLANE('',#5519);
#530=PLANE('',#5520);
#531=PLANE('',#5523);
#532=PLANE('',#5531);
#533=PLANE('',#5532);
#534=PLANE('',#5540);
#535=PLANE('',#5541);
#536=PLANE('',#5549);
#537=PLANE('',#5550);
#538=PLANE('',#5558);
#539=PLANE('',#5559);
#540=PLANE('',#5567);
#541=PLANE('',#5568);
#542=PLANE('',#5584);
#543=PLANE('',#5587);
#544=PLANE('',#5599);
#545=PLANE('',#5608);
#546=PLANE('',#5641);
#547=PLANE('',#5646);
#548=PLANE('',#5651);
#549=PLANE('',#5656);
#550=PLANE('',#5661);
#551=PLANE('',#5666);
#552=PLANE('',#5675);
#553=PLANE('',#5679);
#554=PLANE('',#5680);
#555=PLANE('',#5682);
#556=PLANE('',#5687);
#557=PLANE('',#5690);
#558=PLANE('',#5695);
#559=PLANE('',#5710);
#560=PLANE('',#5711);
#561=PLANE('',#5713);
#562=PLANE('',#5714);
#563=PLANE('',#5716);
#564=PLANE('',#5717);
#565=PLANE('',#5727);
#566=PLANE('',#5728);
#567=PLANE('',#5729);
#568=PLANE('',#5734);
#569=PLANE('',#5735);
#570=PLANE('',#5736);
#571=PLANE('',#5737);
#572=PLANE('',#5738);
#573=PLANE('',#5739);
#574=PLANE('',#5740);
#575=PLANE('',#5741);
#576=PLANE('',#5749);
#577=PLANE('',#5750);
#578=PLANE('',#5751);
#579=PLANE('',#5752);
#580=PLANE('',#5753);
#581=PLANE('',#5754);
#582=PLANE('',#5755);
#583=PLANE('',#5756);
#584=PLANE('',#5764);
#585=PLANE('',#5765);
#586=PLANE('',#5767);
#587=PLANE('',#5768);
#588=PLANE('',#5770);
#589=PLANE('',#5771);
#590=PLANE('',#5781);
#591=PLANE('',#5782);
#592=PLANE('',#5783);
#593=PLANE('',#5788);
#594=PLANE('',#5789);
#595=PLANE('',#5790);
#596=PLANE('',#5791);
#597=PLANE('',#5792);
#598=PLANE('',#5793);
#599=PLANE('',#5794);
#600=PLANE('',#5795);
#601=PLANE('',#5803);
#602=PLANE('',#5804);
#603=PLANE('',#5805);
#604=PLANE('',#5806);
#605=PLANE('',#5807);
#606=PLANE('',#5808);
#607=PLANE('',#5809);
#608=PLANE('',#5810);
#609=PLANE('',#5812);
#610=PLANE('',#5813);
#611=PLANE('',#5814);
#612=PLANE('',#5815);
#613=PLANE('',#5816);
#614=PLANE('',#5817);
#615=PLANE('',#5818);
#616=PLANE('',#5819);
#617=PLANE('',#5820);
#618=PLANE('',#5821);
#619=PLANE('',#5822);
#620=PLANE('',#5823);
#621=PLANE('',#5824);
#622=PLANE('',#5825);
#623=PLANE('',#5826);
#624=PLANE('',#5827);
#625=PLANE('',#5828);
#626=PLANE('',#5829);
#627=PLANE('',#5830);
#628=PLANE('',#5831);
#629=PLANE('',#5832);
#630=PLANE('',#5833);
#631=PLANE('',#5834);
#632=PLANE('',#5835);
#633=PLANE('',#5836);
#634=PLANE('',#5837);
#635=PLANE('',#5838);
#636=PLANE('',#5839);
#637=PLANE('',#5840);
#638=PLANE('',#5841);
#639=PLANE('',#5842);
#640=PLANE('',#5843);
#641=PLANE('',#5844);
#642=PLANE('',#5845);
#643=PLANE('',#5846);
#644=PLANE('',#5847);
#645=PLANE('',#5851);
#646=PLANE('',#5852);
#647=PLANE('',#5853);
#648=PLANE('',#5854);
#649=PLANE('',#5855);
#650=PLANE('',#5856);
#651=PLANE('',#5857);
#652=PLANE('',#5858);
#653=PLANE('',#5859);
#654=PLANE('',#5860);
#655=PLANE('',#5862);
#656=PLANE('',#5870);
#657=PLANE('',#5871);
#658=PLANE('',#5872);
#659=PLANE('',#5873);
#660=PLANE('',#5874);
#661=PLANE('',#5875);
#662=PLANE('',#5876);
#663=PLANE('',#5877);
#664=PLANE('',#5884);
#665=PLANE('',#5888);
#666=PLANE('',#5890);
#667=PLANE('',#5891);
#668=PLANE('',#5892);
#669=PLANE('',#5893);
#670=PLANE('',#5894);
#671=PLANE('',#5895);
#672=PLANE('',#5896);
#673=PLANE('',#5897);
#674=PLANE('',#5898);
#675=PLANE('',#5900);
#676=PLANE('',#5908);
#677=PLANE('',#5919);
#678=PLANE('',#5922);
#679=PLANE('',#5923);
#680=PLANE('',#5924);
#681=PLANE('',#5925);
#682=PLANE('',#5926);
#683=PLANE('',#5927);
#684=PLANE('',#5928);
#685=PLANE('',#5929);
#686=PLANE('',#5935);
#687=PLANE('',#5936);
#688=PLANE('',#5937);
#689=PLANE('',#5941);
#690=PLANE('',#5942);
#691=PLANE('',#5943);
#692=PLANE('',#5944);
#693=PLANE('',#5945);
#694=PLANE('',#5963);
#695=PLANE('',#5970);
#696=PLANE('',#5971);
#697=PLANE('',#5988);
#698=PLANE('',#5995);
#699=PLANE('',#5996);
#700=PLANE('',#6004);
#701=PLANE('',#6005);
#702=PLANE('',#6025);
#703=PLANE('',#6026);
#704=PLANE('',#6028);
#705=PLANE('',#6036);
#706=PLANE('',#6044);
#707=PLANE('',#6045);
#708=PLANE('',#6046);
#709=PLANE('',#6047);
#710=PLANE('',#6048);
#711=PLANE('',#6049);
#712=PLANE('',#6050);
#713=PLANE('',#6051);
#714=PLANE('',#6052);
#715=FACE_OUTER_BOUND('',#1011,.T.);
#716=FACE_OUTER_BOUND('',#1012,.T.);
#717=FACE_OUTER_BOUND('',#1013,.T.);
#718=FACE_OUTER_BOUND('',#1014,.T.);
#719=FACE_OUTER_BOUND('',#1015,.T.);
#720=FACE_OUTER_BOUND('',#1017,.T.);
#721=FACE_OUTER_BOUND('',#1019,.T.);
#722=FACE_OUTER_BOUND('',#1020,.T.);
#723=FACE_OUTER_BOUND('',#1021,.T.);
#724=FACE_OUTER_BOUND('',#1022,.T.);
#725=FACE_OUTER_BOUND('',#1024,.T.);
#726=FACE_OUTER_BOUND('',#1026,.T.);
#727=FACE_OUTER_BOUND('',#1027,.T.);
#728=FACE_OUTER_BOUND('',#1028,.T.);
#729=FACE_OUTER_BOUND('',#1030,.T.);
#730=FACE_OUTER_BOUND('',#1032,.T.);
#731=FACE_OUTER_BOUND('',#1033,.T.);
#732=FACE_OUTER_BOUND('',#1034,.T.);
#733=FACE_OUTER_BOUND('',#1036,.T.);
#734=FACE_OUTER_BOUND('',#1038,.T.);
#735=FACE_OUTER_BOUND('',#1039,.T.);
#736=FACE_OUTER_BOUND('',#1040,.T.);
#737=FACE_OUTER_BOUND('',#1042,.T.);
#738=FACE_OUTER_BOUND('',#1044,.T.);
#739=FACE_OUTER_BOUND('',#1045,.T.);
#740=FACE_OUTER_BOUND('',#1046,.T.);
#741=FACE_OUTER_BOUND('',#1048,.T.);
#742=FACE_OUTER_BOUND('',#1050,.T.);
#743=FACE_OUTER_BOUND('',#1051,.T.);
#744=FACE_OUTER_BOUND('',#1052,.T.);
#745=FACE_OUTER_BOUND('',#1053,.T.);
#746=FACE_OUTER_BOUND('',#1054,.T.);
#747=FACE_OUTER_BOUND('',#1056,.T.);
#748=FACE_OUTER_BOUND('',#1057,.T.);
#749=FACE_OUTER_BOUND('',#1059,.T.);
#750=FACE_OUTER_BOUND('',#1060,.T.);
#751=FACE_OUTER_BOUND('',#1061,.T.);
#752=FACE_OUTER_BOUND('',#1062,.T.);
#753=FACE_OUTER_BOUND('',#1064,.T.);
#754=FACE_OUTER_BOUND('',#1065,.T.);
#755=FACE_OUTER_BOUND('',#1066,.T.);
#756=FACE_OUTER_BOUND('',#1067,.T.);
#757=FACE_OUTER_BOUND('',#1069,.T.);
#758=FACE_OUTER_BOUND('',#1070,.T.);
#759=FACE_OUTER_BOUND('',#1071,.T.);
#760=FACE_OUTER_BOUND('',#1072,.T.);
#761=FACE_OUTER_BOUND('',#1073,.T.);
#762=FACE_OUTER_BOUND('',#1074,.T.);
#763=FACE_OUTER_BOUND('',#1075,.T.);
#764=FACE_OUTER_BOUND('',#1076,.T.);
#765=FACE_OUTER_BOUND('',#1077,.T.);
#766=FACE_OUTER_BOUND('',#1078,.T.);
#767=FACE_OUTER_BOUND('',#1079,.T.);
#768=FACE_OUTER_BOUND('',#1080,.T.);
#769=FACE_OUTER_BOUND('',#1081,.T.);
#770=FACE_OUTER_BOUND('',#1082,.T.);
#771=FACE_OUTER_BOUND('',#1083,.T.);
#772=FACE_OUTER_BOUND('',#1084,.T.);
#773=FACE_OUTER_BOUND('',#1085,.T.);
#774=FACE_OUTER_BOUND('',#1086,.T.);
#775=FACE_OUTER_BOUND('',#1087,.T.);
#776=FACE_OUTER_BOUND('',#1088,.T.);
#777=FACE_OUTER_BOUND('',#1089,.T.);
#778=FACE_OUTER_BOUND('',#1090,.T.);
#779=FACE_OUTER_BOUND('',#1091,.T.);
#780=FACE_OUTER_BOUND('',#1092,.T.);
#781=FACE_OUTER_BOUND('',#1093,.T.);
#782=FACE_OUTER_BOUND('',#1094,.T.);
#783=FACE_OUTER_BOUND('',#1095,.T.);
#784=FACE_OUTER_BOUND('',#1097,.T.);
#785=FACE_OUTER_BOUND('',#1098,.T.);
#786=FACE_OUTER_BOUND('',#1100,.T.);
#787=FACE_OUTER_BOUND('',#1101,.T.);
#788=FACE_OUTER_BOUND('',#1103,.T.);
#789=FACE_OUTER_BOUND('',#1104,.T.);
#790=FACE_OUTER_BOUND('',#1106,.T.);
#791=FACE_OUTER_BOUND('',#1107,.T.);
#792=FACE_OUTER_BOUND('',#1109,.T.);
#793=FACE_OUTER_BOUND('',#1110,.T.);
#794=FACE_OUTER_BOUND('',#1111,.T.);
#795=FACE_OUTER_BOUND('',#1112,.T.);
#796=FACE_OUTER_BOUND('',#1113,.T.);
#797=FACE_OUTER_BOUND('',#1115,.T.);
#798=FACE_OUTER_BOUND('',#1116,.T.);
#799=FACE_OUTER_BOUND('',#1117,.T.);
#800=FACE_OUTER_BOUND('',#1118,.T.);
#801=FACE_OUTER_BOUND('',#1120,.T.);
#802=FACE_OUTER_BOUND('',#1121,.T.);
#803=FACE_OUTER_BOUND('',#1122,.T.);
#804=FACE_OUTER_BOUND('',#1123,.T.);
#805=FACE_OUTER_BOUND('',#1124,.T.);
#806=FACE_OUTER_BOUND('',#1125,.T.);
#807=FACE_OUTER_BOUND('',#1126,.T.);
#808=FACE_OUTER_BOUND('',#1127,.T.);
#809=FACE_OUTER_BOUND('',#1128,.T.);
#810=FACE_OUTER_BOUND('',#1129,.T.);
#811=FACE_OUTER_BOUND('',#1130,.T.);
#812=FACE_OUTER_BOUND('',#1131,.T.);
#813=FACE_OUTER_BOUND('',#1132,.T.);
#814=FACE_OUTER_BOUND('',#1133,.T.);
#815=FACE_OUTER_BOUND('',#1134,.T.);
#816=FACE_OUTER_BOUND('',#1140,.T.);
#817=FACE_OUTER_BOUND('',#1143,.T.);
#818=FACE_OUTER_BOUND('',#1144,.T.);
#819=FACE_OUTER_BOUND('',#1145,.T.);
#820=FACE_OUTER_BOUND('',#1146,.T.);
#821=FACE_OUTER_BOUND('',#1148,.T.);
#822=FACE_OUTER_BOUND('',#1150,.T.);
#823=FACE_OUTER_BOUND('',#1151,.T.);
#824=FACE_OUTER_BOUND('',#1152,.T.);
#825=FACE_OUTER_BOUND('',#1153,.T.);
#826=FACE_OUTER_BOUND('',#1155,.T.);
#827=FACE_OUTER_BOUND('',#1157,.T.);
#828=FACE_OUTER_BOUND('',#1158,.T.);
#829=FACE_OUTER_BOUND('',#1159,.T.);
#830=FACE_OUTER_BOUND('',#1160,.T.);
#831=FACE_OUTER_BOUND('',#1162,.T.);
#832=FACE_OUTER_BOUND('',#1163,.T.);
#833=FACE_OUTER_BOUND('',#1164,.T.);
#834=FACE_OUTER_BOUND('',#1165,.T.);
#835=FACE_OUTER_BOUND('',#1167,.T.);
#836=FACE_OUTER_BOUND('',#1168,.T.);
#837=FACE_OUTER_BOUND('',#1169,.T.);
#838=FACE_OUTER_BOUND('',#1170,.T.);
#839=FACE_OUTER_BOUND('',#1171,.T.);
#840=FACE_OUTER_BOUND('',#1172,.T.);
#841=FACE_OUTER_BOUND('',#1173,.T.);
#842=FACE_OUTER_BOUND('',#1174,.T.);
#843=FACE_OUTER_BOUND('',#1175,.T.);
#844=FACE_OUTER_BOUND('',#1176,.T.);
#845=FACE_OUTER_BOUND('',#1177,.T.);
#846=FACE_OUTER_BOUND('',#1178,.T.);
#847=FACE_OUTER_BOUND('',#1179,.T.);
#848=FACE_OUTER_BOUND('',#1180,.T.);
#849=FACE_OUTER_BOUND('',#1181,.T.);
#850=FACE_OUTER_BOUND('',#1187,.T.);
#851=FACE_OUTER_BOUND('',#1190,.T.);
#852=FACE_OUTER_BOUND('',#1191,.T.);
#853=FACE_OUTER_BOUND('',#1192,.T.);
#854=FACE_OUTER_BOUND('',#1193,.T.);
#855=FACE_OUTER_BOUND('',#1195,.T.);
#856=FACE_OUTER_BOUND('',#1197,.T.);
#857=FACE_OUTER_BOUND('',#1198,.T.);
#858=FACE_OUTER_BOUND('',#1199,.T.);
#859=FACE_OUTER_BOUND('',#1200,.T.);
#860=FACE_OUTER_BOUND('',#1202,.T.);
#861=FACE_OUTER_BOUND('',#1204,.T.);
#862=FACE_OUTER_BOUND('',#1205,.T.);
#863=FACE_OUTER_BOUND('',#1206,.T.);
#864=FACE_OUTER_BOUND('',#1207,.T.);
#865=FACE_OUTER_BOUND('',#1208,.T.);
#866=FACE_OUTER_BOUND('',#1209,.T.);
#867=FACE_OUTER_BOUND('',#1210,.T.);
#868=FACE_OUTER_BOUND('',#1211,.T.);
#869=FACE_OUTER_BOUND('',#1212,.T.);
#870=FACE_OUTER_BOUND('',#1213,.T.);
#871=FACE_OUTER_BOUND('',#1214,.T.);
#872=FACE_OUTER_BOUND('',#1215,.T.);
#873=FACE_OUTER_BOUND('',#1216,.T.);
#874=FACE_OUTER_BOUND('',#1217,.T.);
#875=FACE_OUTER_BOUND('',#1218,.T.);
#876=FACE_OUTER_BOUND('',#1219,.T.);
#877=FACE_OUTER_BOUND('',#1220,.T.);
#878=FACE_OUTER_BOUND('',#1221,.T.);
#879=FACE_OUTER_BOUND('',#1222,.T.);
#880=FACE_OUTER_BOUND('',#1223,.T.);
#881=FACE_OUTER_BOUND('',#1224,.T.);
#882=FACE_OUTER_BOUND('',#1225,.T.);
#883=FACE_OUTER_BOUND('',#1226,.T.);
#884=FACE_OUTER_BOUND('',#1227,.T.);
#885=FACE_OUTER_BOUND('',#1228,.T.);
#886=FACE_OUTER_BOUND('',#1229,.T.);
#887=FACE_OUTER_BOUND('',#1230,.T.);
#888=FACE_OUTER_BOUND('',#1231,.T.);
#889=FACE_OUTER_BOUND('',#1232,.T.);
#890=FACE_OUTER_BOUND('',#1233,.T.);
#891=FACE_OUTER_BOUND('',#1234,.T.);
#892=FACE_OUTER_BOUND('',#1235,.T.);
#893=FACE_OUTER_BOUND('',#1236,.T.);
#894=FACE_OUTER_BOUND('',#1237,.T.);
#895=FACE_OUTER_BOUND('',#1238,.T.);
#896=FACE_OUTER_BOUND('',#1239,.T.);
#897=FACE_OUTER_BOUND('',#1240,.T.);
#898=FACE_OUTER_BOUND('',#1241,.T.);
#899=FACE_OUTER_BOUND('',#1242,.T.);
#900=FACE_OUTER_BOUND('',#1243,.T.);
#901=FACE_OUTER_BOUND('',#1244,.T.);
#902=FACE_OUTER_BOUND('',#1245,.T.);
#903=FACE_OUTER_BOUND('',#1246,.T.);
#904=FACE_OUTER_BOUND('',#1247,.T.);
#905=FACE_OUTER_BOUND('',#1248,.T.);
#906=FACE_OUTER_BOUND('',#1249,.T.);
#907=FACE_OUTER_BOUND('',#1251,.T.);
#908=FACE_OUTER_BOUND('',#1253,.T.);
#909=FACE_OUTER_BOUND('',#1254,.T.);
#910=FACE_OUTER_BOUND('',#1255,.T.);
#911=FACE_OUTER_BOUND('',#1256,.T.);
#912=FACE_OUTER_BOUND('',#1257,.T.);
#913=FACE_OUTER_BOUND('',#1258,.T.);
#914=FACE_OUTER_BOUND('',#1259,.T.);
#915=FACE_OUTER_BOUND('',#1260,.T.);
#916=FACE_OUTER_BOUND('',#1261,.T.);
#917=FACE_OUTER_BOUND('',#1262,.T.);
#918=FACE_OUTER_BOUND('',#1264,.T.);
#919=FACE_OUTER_BOUND('',#1265,.T.);
#920=FACE_OUTER_BOUND('',#1266,.T.);
#921=FACE_OUTER_BOUND('',#1268,.T.);
#922=FACE_OUTER_BOUND('',#1269,.T.);
#923=FACE_OUTER_BOUND('',#1271,.T.);
#924=FACE_OUTER_BOUND('',#1272,.T.);
#925=FACE_OUTER_BOUND('',#1273,.T.);
#926=FACE_OUTER_BOUND('',#1274,.T.);
#927=FACE_OUTER_BOUND('',#1275,.T.);
#928=FACE_OUTER_BOUND('',#1276,.T.);
#929=FACE_OUTER_BOUND('',#1277,.T.);
#930=FACE_OUTER_BOUND('',#1278,.T.);
#931=FACE_OUTER_BOUND('',#1279,.T.);
#932=FACE_OUTER_BOUND('',#1280,.T.);
#933=FACE_OUTER_BOUND('',#1281,.T.);
#934=FACE_OUTER_BOUND('',#1282,.T.);
#935=FACE_OUTER_BOUND('',#1283,.T.);
#936=FACE_OUTER_BOUND('',#1284,.T.);
#937=FACE_OUTER_BOUND('',#1286,.T.);
#938=FACE_OUTER_BOUND('',#1287,.T.);
#939=FACE_OUTER_BOUND('',#1288,.T.);
#940=FACE_OUTER_BOUND('',#1289,.T.);
#941=FACE_OUTER_BOUND('',#1290,.T.);
#942=FACE_OUTER_BOUND('',#1291,.T.);
#943=FACE_OUTER_BOUND('',#1292,.T.);
#944=FACE_OUTER_BOUND('',#1293,.T.);
#945=FACE_OUTER_BOUND('',#1294,.T.);
#946=FACE_OUTER_BOUND('',#1295,.T.);
#947=FACE_OUTER_BOUND('',#1296,.T.);
#948=FACE_OUTER_BOUND('',#1297,.T.);
#949=FACE_OUTER_BOUND('',#1298,.T.);
#950=FACE_OUTER_BOUND('',#1299,.T.);
#951=FACE_OUTER_BOUND('',#1301,.T.);
#952=FACE_OUTER_BOUND('',#1302,.T.);
#953=FACE_OUTER_BOUND('',#1303,.T.);
#954=FACE_OUTER_BOUND('',#1304,.T.);
#955=FACE_OUTER_BOUND('',#1305,.T.);
#956=FACE_OUTER_BOUND('',#1306,.T.);
#957=FACE_OUTER_BOUND('',#1307,.T.);
#958=FACE_OUTER_BOUND('',#1308,.T.);
#959=FACE_OUTER_BOUND('',#1309,.T.);
#960=FACE_OUTER_BOUND('',#1310,.T.);
#961=FACE_OUTER_BOUND('',#1312,.T.);
#962=FACE_OUTER_BOUND('',#1314,.T.);
#963=FACE_OUTER_BOUND('',#1315,.T.);
#964=FACE_OUTER_BOUND('',#1316,.T.);
#965=FACE_OUTER_BOUND('',#1317,.T.);
#966=FACE_OUTER_BOUND('',#1318,.T.);
#967=FACE_OUTER_BOUND('',#1319,.T.);
#968=FACE_OUTER_BOUND('',#1321,.T.);
#969=FACE_OUTER_BOUND('',#1322,.T.);
#970=FACE_OUTER_BOUND('',#1323,.T.);
#971=FACE_OUTER_BOUND('',#1329,.T.);
#972=FACE_OUTER_BOUND('',#1335,.T.);
#973=FACE_OUTER_BOUND('',#1336,.T.);
#974=FACE_OUTER_BOUND('',#1337,.T.);
#975=FACE_OUTER_BOUND('',#1338,.T.);
#976=FACE_OUTER_BOUND('',#1339,.T.);
#977=FACE_OUTER_BOUND('',#1340,.T.);
#978=FACE_OUTER_BOUND('',#1342,.T.);
#979=FACE_OUTER_BOUND('',#1343,.T.);
#980=FACE_OUTER_BOUND('',#1344,.T.);
#981=FACE_OUTER_BOUND('',#1350,.T.);
#982=FACE_OUTER_BOUND('',#1356,.T.);
#983=FACE_OUTER_BOUND('',#1357,.T.);
#984=FACE_OUTER_BOUND('',#1358,.T.);
#985=FACE_OUTER_BOUND('',#1360,.T.);
#986=FACE_OUTER_BOUND('',#1362,.T.);
#987=FACE_OUTER_BOUND('',#1363,.T.);
#988=FACE_OUTER_BOUND('',#1364,.T.);
#989=FACE_OUTER_BOUND('',#1365,.T.);
#990=FACE_OUTER_BOUND('',#1366,.T.);
#991=FACE_OUTER_BOUND('',#1367,.T.);
#992=FACE_OUTER_BOUND('',#1368,.T.);
#993=FACE_OUTER_BOUND('',#1374,.T.);
#994=FACE_OUTER_BOUND('',#1380,.T.);
#995=FACE_OUTER_BOUND('',#1381,.T.);
#996=FACE_OUTER_BOUND('',#1382,.T.);
#997=FACE_OUTER_BOUND('',#1383,.T.);
#998=FACE_OUTER_BOUND('',#1384,.T.);
#999=FACE_OUTER_BOUND('',#1386,.T.);
#1000=FACE_OUTER_BOUND('',#1387,.T.);
#1001=FACE_OUTER_BOUND('',#1388,.T.);
#1002=FACE_OUTER_BOUND('',#1389,.T.);
#1003=FACE_OUTER_BOUND('',#1390,.T.);
#1004=FACE_OUTER_BOUND('',#1391,.T.);
#1005=FACE_OUTER_BOUND('',#1392,.T.);
#1006=FACE_OUTER_BOUND('',#1393,.T.);
#1007=FACE_OUTER_BOUND('',#1394,.T.);
#1008=FACE_OUTER_BOUND('',#1395,.T.);
#1009=FACE_OUTER_BOUND('',#1396,.T.);
#1010=FACE_OUTER_BOUND('',#1397,.T.);
#1011=EDGE_LOOP('',(#3517,#3518,#3519,#3520));
#1012=EDGE_LOOP('',(#3521));
#1013=EDGE_LOOP('',(#3522,#3523,#3524,#3525));
#1014=EDGE_LOOP('',(#3526));
#1015=EDGE_LOOP('',(#3527));
#1016=EDGE_LOOP('',(#3528));
#1017=EDGE_LOOP('',(#3529));
#1018=EDGE_LOOP('',(#3530));
#1019=EDGE_LOOP('',(#3531,#3532,#3533,#3534));
#1020=EDGE_LOOP('',(#3535,#3536,#3537,#3538));
#1021=EDGE_LOOP('',(#3539,#3540,#3541,#3542));
#1022=EDGE_LOOP('',(#3543));
#1023=EDGE_LOOP('',(#3544));
#1024=EDGE_LOOP('',(#3545));
#1025=EDGE_LOOP('',(#3546));
#1026=EDGE_LOOP('',(#3547,#3548,#3549,#3550));
#1027=EDGE_LOOP('',(#3551,#3552,#3553,#3554));
#1028=EDGE_LOOP('',(#3555));
#1029=EDGE_LOOP('',(#3556));
#1030=EDGE_LOOP('',(#3557));
#1031=EDGE_LOOP('',(#3558));
#1032=EDGE_LOOP('',(#3559,#3560,#3561,#3562));
#1033=EDGE_LOOP('',(#3563,#3564,#3565,#3566));
#1034=EDGE_LOOP('',(#3567));
#1035=EDGE_LOOP('',(#3568));
#1036=EDGE_LOOP('',(#3569));
#1037=EDGE_LOOP('',(#3570));
#1038=EDGE_LOOP('',(#3571,#3572,#3573,#3574));
#1039=EDGE_LOOP('',(#3575,#3576,#3577,#3578));
#1040=EDGE_LOOP('',(#3579));
#1041=EDGE_LOOP('',(#3580));
#1042=EDGE_LOOP('',(#3581));
#1043=EDGE_LOOP('',(#3582));
#1044=EDGE_LOOP('',(#3583,#3584,#3585,#3586));
#1045=EDGE_LOOP('',(#3587,#3588,#3589,#3590));
#1046=EDGE_LOOP('',(#3591));
#1047=EDGE_LOOP('',(#3592));
#1048=EDGE_LOOP('',(#3593));
#1049=EDGE_LOOP('',(#3594));
#1050=EDGE_LOOP('',(#3595,#3596,#3597,#3598,#3599,#3600));
#1051=EDGE_LOOP('',(#3601,#3602,#3603,#3604,#3605));
#1052=EDGE_LOOP('',(#3606,#3607,#3608,#3609));
#1053=EDGE_LOOP('',(#3610,#3611,#3612,#3613));
#1054=EDGE_LOOP('',(#3614));
#1055=EDGE_LOOP('',(#3615));
#1056=EDGE_LOOP('',(#3616,#3617,#3618,#3619,#3620));
#1057=EDGE_LOOP('',(#3621));
#1058=EDGE_LOOP('',(#3622));
#1059=EDGE_LOOP('',(#3623,#3624,#3625,#3626));
#1060=EDGE_LOOP('',(#3627,#3628,#3629,#3630,#3631,#3632));
#1061=EDGE_LOOP('',(#3633,#3634,#3635,#3636,#3637));
#1062=EDGE_LOOP('',(#3638));
#1063=EDGE_LOOP('',(#3639));
#1064=EDGE_LOOP('',(#3640,#3641,#3642,#3643));
#1065=EDGE_LOOP('',(#3644,#3645,#3646,#3647));
#1066=EDGE_LOOP('',(#3648,#3649,#3650,#3651));
#1067=EDGE_LOOP('',(#3652));
#1068=EDGE_LOOP('',(#3653));
#1069=EDGE_LOOP('',(#3654,#3655,#3656,#3657,#3658));
#1070=EDGE_LOOP('',(#3659,#3660));
#1071=EDGE_LOOP('',(#3661,#3662));
#1072=EDGE_LOOP('',(#3663,#3664));
#1073=EDGE_LOOP('',(#3665,#3666));
#1074=EDGE_LOOP('',(#3667,#3668));
#1075=EDGE_LOOP('',(#3669,#3670));
#1076=EDGE_LOOP('',(#3671,#3672));
#1077=EDGE_LOOP('',(#3673,#3674));
#1078=EDGE_LOOP('',(#3675,#3676,#3677,#3678));
#1079=EDGE_LOOP('',(#3679,#3680,#3681,#3682,#3683,#3684,#3685,#3686,#3687,
#3688,#3689,#3690,#3691,#3692,#3693,#3694,#3695,#3696,#3697,#3698));
#1080=EDGE_LOOP('',(#3699,#3700,#3701,#3702));
#1081=EDGE_LOOP('',(#3703,#3704,#3705,#3706));
#1082=EDGE_LOOP('',(#3707,#3708,#3709,#3710));
#1083=EDGE_LOOP('',(#3711,#3712,#3713,#3714));
#1084=EDGE_LOOP('',(#3715,#3716,#3717,#3718));
#1085=EDGE_LOOP('',(#3719,#3720,#3721,#3722,#3723,#3724));
#1086=EDGE_LOOP('',(#3725,#3726,#3727,#3728));
#1087=EDGE_LOOP('',(#3729,#3730,#3731,#3732));
#1088=EDGE_LOOP('',(#3733,#3734,#3735,#3736));
#1089=EDGE_LOOP('',(#3737,#3738,#3739,#3740));
#1090=EDGE_LOOP('',(#3741,#3742,#3743,#3744));
#1091=EDGE_LOOP('',(#3745,#3746,#3747,#3748));
#1092=EDGE_LOOP('',(#3749,#3750,#3751,#3752,#3753,#3754,#3755,#3756,#3757,
#3758,#3759,#3760,#3761,#3762,#3763,#3764,#3765,#3766,#3767,#3768));
#1093=EDGE_LOOP('',(#3769,#3770,#3771,#3772));
#1094=EDGE_LOOP('',(#3773,#3774,#3775,#3776));
#1095=EDGE_LOOP('',(#3777));
#1096=EDGE_LOOP('',(#3778));
#1097=EDGE_LOOP('',(#3779,#3780,#3781,#3782));
#1098=EDGE_LOOP('',(#3783));
#1099=EDGE_LOOP('',(#3784));
#1100=EDGE_LOOP('',(#3785,#3786,#3787,#3788));
#1101=EDGE_LOOP('',(#3789));
#1102=EDGE_LOOP('',(#3790));
#1103=EDGE_LOOP('',(#3791,#3792,#3793,#3794));
#1104=EDGE_LOOP('',(#3795));
#1105=EDGE_LOOP('',(#3796));
#1106=EDGE_LOOP('',(#3797,#3798,#3799,#3800));
#1107=EDGE_LOOP('',(#3801));
#1108=EDGE_LOOP('',(#3802));
#1109=EDGE_LOOP('',(#3803,#3804,#3805,#3806));
#1110=EDGE_LOOP('',(#3807,#3808,#3809,#3810));
#1111=EDGE_LOOP('',(#3811,#3812,#3813,#3814));
#1112=EDGE_LOOP('',(#3815,#3816,#3817,#3818));
#1113=EDGE_LOOP('',(#3819,#3820,#3821,#3822));
#1114=EDGE_LOOP('',(#3823));
#1115=EDGE_LOOP('',(#3824,#3825,#3826,#3827));
#1116=EDGE_LOOP('',(#3828,#3829,#3830,#3831));
#1117=EDGE_LOOP('',(#3832,#3833,#3834,#3835));
#1118=EDGE_LOOP('',(#3836,#3837,#3838,#3839));
#1119=EDGE_LOOP('',(#3840));
#1120=EDGE_LOOP('',(#3841,#3842,#3843,#3844));
#1121=EDGE_LOOP('',(#3845,#3846,#3847,#3848));
#1122=EDGE_LOOP('',(#3849,#3850,#3851,#3852));
#1123=EDGE_LOOP('',(#3853,#3854,#3855,#3856));
#1124=EDGE_LOOP('',(#3857,#3858,#3859,#3860));
#1125=EDGE_LOOP('',(#3861,#3862,#3863,#3864));
#1126=EDGE_LOOP('',(#3865,#3866,#3867,#3868));
#1127=EDGE_LOOP('',(#3869,#3870,#3871,#3872));
#1128=EDGE_LOOP('',(#3873,#3874,#3875,#3876));
#1129=EDGE_LOOP('',(#3877,#3878,#3879,#3880));
#1130=EDGE_LOOP('',(#3881,#3882,#3883,#3884));
#1131=EDGE_LOOP('',(#3885,#3886,#3887,#3888));
#1132=EDGE_LOOP('',(#3889,#3890,#3891,#3892));
#1133=EDGE_LOOP('',(#3893,#3894,#3895,#3896));
#1134=EDGE_LOOP('',(#3897,#3898,#3899,#3900));
#1135=EDGE_LOOP('',(#3901,#3902,#3903,#3904));
#1136=EDGE_LOOP('',(#3905));
#1137=EDGE_LOOP('',(#3906,#3907,#3908,#3909));
#1138=EDGE_LOOP('',(#3910));
#1139=EDGE_LOOP('',(#3911,#3912,#3913,#3914));
#1140=EDGE_LOOP('',(#3915,#3916,#3917,#3918));
#1141=EDGE_LOOP('',(#3919));
#1142=EDGE_LOOP('',(#3920));
#1143=EDGE_LOOP('',(#3921,#3922,#3923,#3924));
#1144=EDGE_LOOP('',(#3925,#3926,#3927,#3928));
#1145=EDGE_LOOP('',(#3929,#3930,#3931,#3932));
#1146=EDGE_LOOP('',(#3933,#3934,#3935,#3936));
#1147=EDGE_LOOP('',(#3937));
#1148=EDGE_LOOP('',(#3938,#3939,#3940,#3941));
#1149=EDGE_LOOP('',(#3942));
#1150=EDGE_LOOP('',(#3943,#3944,#3945,#3946,#3947,#3948));
#1151=EDGE_LOOP('',(#3949,#3950,#3951,#3952,#3953,#3954));
#1152=EDGE_LOOP('',(#3955,#3956,#3957,#3958));
#1153=EDGE_LOOP('',(#3959,#3960,#3961,#3962));
#1154=EDGE_LOOP('',(#3963));
#1155=EDGE_LOOP('',(#3964,#3965,#3966,#3967));
#1156=EDGE_LOOP('',(#3968));
#1157=EDGE_LOOP('',(#3969,#3970,#3971,#3972));
#1158=EDGE_LOOP('',(#3973,#3974,#3975,#3976));
#1159=EDGE_LOOP('',(#3977,#3978,#3979,#3980));
#1160=EDGE_LOOP('',(#3981,#3982,#3983,#3984));
#1161=EDGE_LOOP('',(#3985));
#1162=EDGE_LOOP('',(#3986,#3987,#3988,#3989));
#1163=EDGE_LOOP('',(#3990,#3991,#3992,#3993));
#1164=EDGE_LOOP('',(#3994,#3995,#3996,#3997));
#1165=EDGE_LOOP('',(#3998,#3999,#4000,#4001));
#1166=EDGE_LOOP('',(#4002));
#1167=EDGE_LOOP('',(#4003,#4004,#4005,#4006));
#1168=EDGE_LOOP('',(#4007,#4008,#4009,#4010));
#1169=EDGE_LOOP('',(#4011,#4012,#4013,#4014));
#1170=EDGE_LOOP('',(#4015,#4016,#4017,#4018));
#1171=EDGE_LOOP('',(#4019,#4020,#4021,#4022));
#1172=EDGE_LOOP('',(#4023,#4024,#4025,#4026));
#1173=EDGE_LOOP('',(#4027,#4028,#4029,#4030));
#1174=EDGE_LOOP('',(#4031,#4032,#4033,#4034));
#1175=EDGE_LOOP('',(#4035,#4036,#4037,#4038));
#1176=EDGE_LOOP('',(#4039,#4040,#4041,#4042));
#1177=EDGE_LOOP('',(#4043,#4044,#4045,#4046));
#1178=EDGE_LOOP('',(#4047,#4048,#4049,#4050));
#1179=EDGE_LOOP('',(#4051,#4052,#4053,#4054));
#1180=EDGE_LOOP('',(#4055,#4056,#4057,#4058));
#1181=EDGE_LOOP('',(#4059,#4060,#4061,#4062));
#1182=EDGE_LOOP('',(#4063,#4064,#4065,#4066));
#1183=EDGE_LOOP('',(#4067));
#1184=EDGE_LOOP('',(#4068,#4069,#4070,#4071));
#1185=EDGE_LOOP('',(#4072));
#1186=EDGE_LOOP('',(#4073,#4074,#4075,#4076));
#1187=EDGE_LOOP('',(#4077,#4078,#4079,#4080));
#1188=EDGE_LOOP('',(#4081));
#1189=EDGE_LOOP('',(#4082));
#1190=EDGE_LOOP('',(#4083,#4084,#4085,#4086));
#1191=EDGE_LOOP('',(#4087,#4088,#4089,#4090));
#1192=EDGE_LOOP('',(#4091,#4092,#4093,#4094));
#1193=EDGE_LOOP('',(#4095,#4096,#4097,#4098));
#1194=EDGE_LOOP('',(#4099));
#1195=EDGE_LOOP('',(#4100,#4101,#4102,#4103));
#1196=EDGE_LOOP('',(#4104));
#1197=EDGE_LOOP('',(#4105,#4106,#4107,#4108,#4109,#4110));
#1198=EDGE_LOOP('',(#4111,#4112,#4113,#4114,#4115,#4116));
#1199=EDGE_LOOP('',(#4117,#4118,#4119,#4120));
#1200=EDGE_LOOP('',(#4121,#4122,#4123,#4124));
#1201=EDGE_LOOP('',(#4125));
#1202=EDGE_LOOP('',(#4126,#4127,#4128,#4129));
#1203=EDGE_LOOP('',(#4130));
#1204=EDGE_LOOP('',(#4131,#4132,#4133,#4134));
#1205=EDGE_LOOP('',(#4135,#4136,#4137,#4138));
#1206=EDGE_LOOP('',(#4139,#4140,#4141,#4142));
#1207=EDGE_LOOP('',(#4143,#4144,#4145,#4146));
#1208=EDGE_LOOP('',(#4147,#4148,#4149,#4150));
#1209=EDGE_LOOP('',(#4151,#4152,#4153,#4154));
#1210=EDGE_LOOP('',(#4155,#4156,#4157,#4158));
#1211=EDGE_LOOP('',(#4159,#4160,#4161,#4162));
#1212=EDGE_LOOP('',(#4163,#4164,#4165,#4166));
#1213=EDGE_LOOP('',(#4167,#4168,#4169,#4170));
#1214=EDGE_LOOP('',(#4171,#4172,#4173,#4174));
#1215=EDGE_LOOP('',(#4175,#4176,#4177,#4178));
#1216=EDGE_LOOP('',(#4179,#4180,#4181,#4182));
#1217=EDGE_LOOP('',(#4183,#4184,#4185,#4186));
#1218=EDGE_LOOP('',(#4187,#4188,#4189,#4190));
#1219=EDGE_LOOP('',(#4191,#4192,#4193,#4194));
#1220=EDGE_LOOP('',(#4195,#4196,#4197,#4198));
#1221=EDGE_LOOP('',(#4199,#4200,#4201,#4202));
#1222=EDGE_LOOP('',(#4203,#4204,#4205,#4206));
#1223=EDGE_LOOP('',(#4207,#4208,#4209,#4210));
#1224=EDGE_LOOP('',(#4211,#4212,#4213,#4214));
#1225=EDGE_LOOP('',(#4215,#4216,#4217,#4218));
#1226=EDGE_LOOP('',(#4219,#4220,#4221,#4222));
#1227=EDGE_LOOP('',(#4223,#4224,#4225,#4226));
#1228=EDGE_LOOP('',(#4227,#4228,#4229,#4230));
#1229=EDGE_LOOP('',(#4231,#4232,#4233,#4234));
#1230=EDGE_LOOP('',(#4235,#4236,#4237,#4238));
#1231=EDGE_LOOP('',(#4239,#4240,#4241,#4242));
#1232=EDGE_LOOP('',(#4243,#4244,#4245,#4246));
#1233=EDGE_LOOP('',(#4247,#4248,#4249,#4250));
#1234=EDGE_LOOP('',(#4251,#4252,#4253,#4254));
#1235=EDGE_LOOP('',(#4255,#4256,#4257,#4258));
#1236=EDGE_LOOP('',(#4259,#4260,#4261,#4262));
#1237=EDGE_LOOP('',(#4263,#4264,#4265,#4266));
#1238=EDGE_LOOP('',(#4267,#4268,#4269,#4270));
#1239=EDGE_LOOP('',(#4271,#4272,#4273,#4274));
#1240=EDGE_LOOP('',(#4275,#4276,#4277,#4278));
#1241=EDGE_LOOP('',(#4279,#4280,#4281,#4282));
#1242=EDGE_LOOP('',(#4283,#4284,#4285,#4286));
#1243=EDGE_LOOP('',(#4287,#4288,#4289,#4290));
#1244=EDGE_LOOP('',(#4291,#4292,#4293,#4294));
#1245=EDGE_LOOP('',(#4295,#4296,#4297,#4298));
#1246=EDGE_LOOP('',(#4299,#4300,#4301,#4302));
#1247=EDGE_LOOP('',(#4303,#4304,#4305,#4306));
#1248=EDGE_LOOP('',(#4307,#4308,#4309,#4310));
#1249=EDGE_LOOP('',(#4311,#4312,#4313,#4314,#4315,#4316,#4317,#4318,#4319,
#4320,#4321,#4322,#4323,#4324,#4325,#4326,#4327,#4328,#4329,#4330,#4331,
#4332,#4333,#4334,#4335,#4336,#4337,#4338,#4339,#4340,#4341,#4342,#4343,
#4344,#4345,#4346,#4347,#4348,#4349,#4350,#4351,#4352,#4353,#4354));
#1250=EDGE_LOOP('',(#4355));
#1251=EDGE_LOOP('',(#4356,#4357,#4358,#4359,#4360,#4361,#4362,#4363,#4364,
#4365,#4366,#4367,#4368,#4369,#4370,#4371,#4372,#4373,#4374,#4375,#4376,
#4377,#4378,#4379,#4380,#4381,#4382,#4383,#4384,#4385,#4386,#4387,#4388,
#4389,#4390,#4391,#4392,#4393,#4394,#4395,#4396,#4397,#4398,#4399));
#1252=EDGE_LOOP('',(#4400));
#1253=EDGE_LOOP('',(#4401,#4402,#4403,#4404,#4405,#4406));
#1254=EDGE_LOOP('',(#4407,#4408,#4409,#4410,#4411,#4412,#4413,#4414));
#1255=EDGE_LOOP('',(#4415,#4416,#4417,#4418,#4419));
#1256=EDGE_LOOP('',(#4420,#4421,#4422,#4423));
#1257=EDGE_LOOP('',(#4424,#4425,#4426,#4427,#4428,#4429));
#1258=EDGE_LOOP('',(#4430,#4431,#4432,#4433,#4434,#4435));
#1259=EDGE_LOOP('',(#4436,#4437,#4438,#4439));
#1260=EDGE_LOOP('',(#4440,#4441,#4442,#4443));
#1261=EDGE_LOOP('',(#4444,#4445,#4446,#4447,#4448,#4449));
#1262=EDGE_LOOP('',(#4450,#4451,#4452,#4453));
#1263=EDGE_LOOP('',(#4454));
#1264=EDGE_LOOP('',(#4455,#4456,#4457,#4458));
#1265=EDGE_LOOP('',(#4459,#4460,#4461,#4462));
#1266=EDGE_LOOP('',(#4463));
#1267=EDGE_LOOP('',(#4464));
#1268=EDGE_LOOP('',(#4465,#4466,#4467,#4468));
#1269=EDGE_LOOP('',(#4469));
#1270=EDGE_LOOP('',(#4470));
#1271=EDGE_LOOP('',(#4471,#4472,#4473,#4474));
#1272=EDGE_LOOP('',(#4475,#4476,#4477,#4478));
#1273=EDGE_LOOP('',(#4479,#4480,#4481,#4482));
#1274=EDGE_LOOP('',(#4483,#4484,#4485,#4486));
#1275=EDGE_LOOP('',(#4487,#4488,#4489,#4490));
#1276=EDGE_LOOP('',(#4491,#4492,#4493,#4494));
#1277=EDGE_LOOP('',(#4495,#4496,#4497,#4498,#4499,#4500));
#1278=EDGE_LOOP('',(#4501,#4502,#4503,#4504,#4505,#4506));
#1279=EDGE_LOOP('',(#4507));
#1280=EDGE_LOOP('',(#4508));
#1281=EDGE_LOOP('',(#4509,#4510,#4511,#4512));
#1282=EDGE_LOOP('',(#4513,#4514,#4515,#4516));
#1283=EDGE_LOOP('',(#4517,#4518,#4519,#4520));
#1284=EDGE_LOOP('',(#4521));
#1285=EDGE_LOOP('',(#4522));
#1286=EDGE_LOOP('',(#4523,#4524,#4525,#4526));
#1287=EDGE_LOOP('',(#4527,#4528,#4529,#4530));
#1288=EDGE_LOOP('',(#4531,#4532,#4533,#4534));
#1289=EDGE_LOOP('',(#4535,#4536,#4537,#4538));
#1290=EDGE_LOOP('',(#4539));
#1291=EDGE_LOOP('',(#4540,#4541,#4542,#4543,#4544,#4545,#4546,#4547,#4548));
#1292=EDGE_LOOP('',(#4549,#4550,#4551,#4552));
#1293=EDGE_LOOP('',(#4553,#4554,#4555,#4556));
#1294=EDGE_LOOP('',(#4557,#4558,#4559,#4560));
#1295=EDGE_LOOP('',(#4561,#4562,#4563,#4564));
#1296=EDGE_LOOP('',(#4565,#4566,#4567,#4568));
#1297=EDGE_LOOP('',(#4569,#4570,#4571,#4572));
#1298=EDGE_LOOP('',(#4573));
#1299=EDGE_LOOP('',(#4574,#4575,#4576,#4577,#4578,#4579));
#1300=EDGE_LOOP('',(#4580));
#1301=EDGE_LOOP('',(#4581,#4582,#4583,#4584,#4585,#4586,#4587,#4588,#4589));
#1302=EDGE_LOOP('',(#4590,#4591,#4592,#4593,#4594,#4595,#4596,#4597,#4598));
#1303=EDGE_LOOP('',(#4599,#4600,#4601,#4602));
#1304=EDGE_LOOP('',(#4603,#4604,#4605,#4606));
#1305=EDGE_LOOP('',(#4607,#4608,#4609,#4610));
#1306=EDGE_LOOP('',(#4611,#4612,#4613,#4614));
#1307=EDGE_LOOP('',(#4615,#4616,#4617,#4618));
#1308=EDGE_LOOP('',(#4619,#4620,#4621,#4622));
#1309=EDGE_LOOP('',(#4623,#4624,#4625,#4626));
#1310=EDGE_LOOP('',(#4627));
#1311=EDGE_LOOP('',(#4628));
#1312=EDGE_LOOP('',(#4629));
#1313=EDGE_LOOP('',(#4630));
#1314=EDGE_LOOP('',(#4631,#4632,#4633,#4634));
#1315=EDGE_LOOP('',(#4635,#4636,#4637,#4638));
#1316=EDGE_LOOP('',(#4639,#4640,#4641,#4642));
#1317=EDGE_LOOP('',(#4643,#4644,#4645,#4646));
#1318=EDGE_LOOP('',(#4647,#4648,#4649,#4650));
#1319=EDGE_LOOP('',(#4651));
#1320=EDGE_LOOP('',(#4652));
#1321=EDGE_LOOP('',(#4653,#4654,#4655,#4656));
#1322=EDGE_LOOP('',(#4657,#4658,#4659,#4660));
#1323=EDGE_LOOP('',(#4661));
#1324=EDGE_LOOP('',(#4662));
#1325=EDGE_LOOP('',(#4663));
#1326=EDGE_LOOP('',(#4664));
#1327=EDGE_LOOP('',(#4665));
#1328=EDGE_LOOP('',(#4666));
#1329=EDGE_LOOP('',(#4667));
#1330=EDGE_LOOP('',(#4668));
#1331=EDGE_LOOP('',(#4669));
#1332=EDGE_LOOP('',(#4670));
#1333=EDGE_LOOP('',(#4671));
#1334=EDGE_LOOP('',(#4672));
#1335=EDGE_LOOP('',(#4673,#4674,#4675,#4676));
#1336=EDGE_LOOP('',(#4677,#4678,#4679,#4680));
#1337=EDGE_LOOP('',(#4681,#4682,#4683,#4684));
#1338=EDGE_LOOP('',(#4685,#4686,#4687,#4688));
#1339=EDGE_LOOP('',(#4689,#4690,#4691,#4692));
#1340=EDGE_LOOP('',(#4693));
#1341=EDGE_LOOP('',(#4694));
#1342=EDGE_LOOP('',(#4695,#4696,#4697,#4698));
#1343=EDGE_LOOP('',(#4699,#4700,#4701,#4702));
#1344=EDGE_LOOP('',(#4703));
#1345=EDGE_LOOP('',(#4704));
#1346=EDGE_LOOP('',(#4705));
#1347=EDGE_LOOP('',(#4706));
#1348=EDGE_LOOP('',(#4707));
#1349=EDGE_LOOP('',(#4708));
#1350=EDGE_LOOP('',(#4709));
#1351=EDGE_LOOP('',(#4710));
#1352=EDGE_LOOP('',(#4711));
#1353=EDGE_LOOP('',(#4712));
#1354=EDGE_LOOP('',(#4713));
#1355=EDGE_LOOP('',(#4714));
#1356=EDGE_LOOP('',(#4715,#4716,#4717,#4718));
#1357=EDGE_LOOP('',(#4719,#4720,#4721,#4722));
#1358=EDGE_LOOP('',(#4723));
#1359=EDGE_LOOP('',(#4724));
#1360=EDGE_LOOP('',(#4725));
#1361=EDGE_LOOP('',(#4726));
#1362=EDGE_LOOP('',(#4727,#4728,#4729,#4730));
#1363=EDGE_LOOP('',(#4731,#4732,#4733,#4734));
#1364=EDGE_LOOP('',(#4735,#4736,#4737,#4738));
#1365=EDGE_LOOP('',(#4739,#4740,#4741,#4742));
#1366=EDGE_LOOP('',(#4743,#4744,#4745,#4746));
#1367=EDGE_LOOP('',(#4747,#4748,#4749,#4750));
#1368=EDGE_LOOP('',(#4751));
#1369=EDGE_LOOP('',(#4752));
#1370=EDGE_LOOP('',(#4753));
#1371=EDGE_LOOP('',(#4754));
#1372=EDGE_LOOP('',(#4755));
#1373=EDGE_LOOP('',(#4756));
#1374=EDGE_LOOP('',(#4757));
#1375=EDGE_LOOP('',(#4758));
#1376=EDGE_LOOP('',(#4759));
#1377=EDGE_LOOP('',(#4760));
#1378=EDGE_LOOP('',(#4761));
#1379=EDGE_LOOP('',(#4762));
#1380=EDGE_LOOP('',(#4763));
#1381=EDGE_LOOP('',(#4764,#4765,#4766,#4767));
#1382=EDGE_LOOP('',(#4768,#4769,#4770,#4771));
#1383=EDGE_LOOP('',(#4772,#4773,#4774,#4775));
#1384=EDGE_LOOP('',(#4776));
#1385=EDGE_LOOP('',(#4777));
#1386=EDGE_LOOP('',(#4778,#4779,#4780,#4781));
#1387=EDGE_LOOP('',(#4782,#4783,#4784,#4785));
#1388=EDGE_LOOP('',(#4786,#4787,#4788,#4789));
#1389=EDGE_LOOP('',(#4790));
#1390=EDGE_LOOP('',(#4791,#4792,#4793,#4794));
#1391=EDGE_LOOP('',(#4795,#4796,#4797,#4798));
#1392=EDGE_LOOP('',(#4799,#4800,#4801,#4802));
#1393=EDGE_LOOP('',(#4803,#4804,#4805,#4806));
#1394=EDGE_LOOP('',(#4807,#4808,#4809,#4810));
#1395=EDGE_LOOP('',(#4811,#4812,#4813,#4814));
#1396=EDGE_LOOP('',(#4815,#4816,#4817,#4818,#4819,#4820));
#1397=EDGE_LOOP('',(#4821,#4822,#4823,#4824,#4825,#4826));
#1398=LINE('',#7715,#1803);
#1399=LINE('',#7722,#1804);
#1400=LINE('',#7736,#1805);
#1401=LINE('',#7739,#1806);
#1402=LINE('',#7744,#1807);
#1403=LINE('',#7752,#1808);
#1404=LINE('',#7758,#1809);
#1405=LINE('',#7767,#1810);
#1406=LINE('',#7773,#1811);
#1407=LINE('',#7782,#1812);
#1408=LINE('',#7788,#1813);
#1409=LINE('',#7797,#1814);
#1410=LINE('',#7803,#1815);
#1411=LINE('',#7821,#1816);
#1412=LINE('',#7827,#1817);
#1413=LINE('',#7831,#1818);
#1414=LINE('',#7837,#1819);
#1415=LINE('',#7842,#1820);
#1416=LINE('',#7857,#1821);
#1417=LINE('',#7866,#1822);
#1418=LINE('',#7870,#1823);
#1419=LINE('',#7874,#1824);
#1420=LINE('',#7877,#1825);
#1421=LINE('',#8030,#1826);
#1422=LINE('',#8326,#1827);
#1423=LINE('',#8368,#1828);
#1424=LINE('',#8373,#1829);
#1425=LINE('',#8382,#1830);
#1426=LINE('',#8387,#1831);
#1427=LINE('',#8397,#1832);
#1428=LINE('',#8401,#1833);
#1429=LINE('',#8406,#1834);
#1430=LINE('',#8410,#1835);
#1431=LINE('',#8414,#1836);
#1432=LINE('',#8416,#1837);
#1433=LINE('',#8417,#1838);
#1434=LINE('',#8420,#1839);
#1435=LINE('',#8422,#1840);
#1436=LINE('',#8423,#1841);
#1437=LINE('',#8428,#1842);
#1438=LINE('',#8429,#1843);
#1439=LINE('',#8432,#1844);
#1440=LINE('',#8436,#1845);
#1441=LINE('',#8437,#1846);
#1442=LINE('',#8440,#1847);
#1443=LINE('',#8441,#1848);
#1444=LINE('',#8448,#1849);
#1445=LINE('',#8453,#1850);
#1446=LINE('',#8457,#1851);
#1447=LINE('',#8463,#1852);
#1448=LINE('',#8465,#1853);
#1449=LINE('',#8466,#1854);
#1450=LINE('',#8469,#1855);
#1451=LINE('',#8470,#1856);
#1452=LINE('',#8473,#1857);
#1453=LINE('',#8474,#1858);
#1454=LINE('',#8479,#1859);
#1455=LINE('',#8482,#1860);
#1456=LINE('',#8484,#1861);
#1457=LINE('',#8486,#1862);
#1458=LINE('',#8490,#1863);
#1459=LINE('',#8492,#1864);
#1460=LINE('',#8494,#1865);
#1461=LINE('',#8495,#1866);
#1462=LINE('',#8498,#1867);
#1463=LINE('',#8500,#1868);
#1464=LINE('',#8501,#1869);
#1465=LINE('',#8504,#1870);
#1466=LINE('',#8506,#1871);
#1467=LINE('',#8507,#1872);
#1468=LINE('',#8509,#1873);
#1469=LINE('',#8510,#1874);
#1470=LINE('',#8518,#1875);
#1471=LINE('',#8524,#1876);
#1472=LINE('',#8529,#1877);
#1473=LINE('',#8531,#1878);
#1474=LINE('',#8533,#1879);
#1475=LINE('',#8534,#1880);
#1476=LINE('',#8538,#1881);
#1477=LINE('',#8539,#1882);
#1478=LINE('',#8540,#1883);
#1479=LINE('',#8543,#1884);
#1480=LINE('',#8545,#1885);
#1481=LINE('',#8546,#1886);
#1482=LINE('',#8549,#1887);
#1483=LINE('',#8551,#1888);
#1484=LINE('',#8552,#1889);
#1485=LINE('',#8555,#1890);
#1486=LINE('',#8557,#1891);
#1487=LINE('',#8558,#1892);
#1488=LINE('',#8560,#1893);
#1489=LINE('',#8562,#1894);
#1490=LINE('',#8568,#1895);
#1491=LINE('',#8572,#1896);
#1492=LINE('',#8577,#1897);
#1493=LINE('',#8581,#1898);
#1494=LINE('',#8585,#1899);
#1495=LINE('',#8587,#1900);
#1496=LINE('',#8588,#1901);
#1497=LINE('',#8591,#1902);
#1498=LINE('',#8593,#1903);
#1499=LINE('',#8594,#1904);
#1500=LINE('',#8599,#1905);
#1501=LINE('',#8600,#1906);
#1502=LINE('',#8603,#1907);
#1503=LINE('',#8607,#1908);
#1504=LINE('',#8608,#1909);
#1505=LINE('',#8611,#1910);
#1506=LINE('',#8612,#1911);
#1507=LINE('',#8619,#1912);
#1508=LINE('',#8624,#1913);
#1509=LINE('',#8628,#1914);
#1510=LINE('',#8634,#1915);
#1511=LINE('',#8636,#1916);
#1512=LINE('',#8637,#1917);
#1513=LINE('',#8640,#1918);
#1514=LINE('',#8641,#1919);
#1515=LINE('',#8644,#1920);
#1516=LINE('',#8645,#1921);
#1517=LINE('',#8650,#1922);
#1518=LINE('',#8653,#1923);
#1519=LINE('',#8655,#1924);
#1520=LINE('',#8657,#1925);
#1521=LINE('',#8661,#1926);
#1522=LINE('',#8663,#1927);
#1523=LINE('',#8665,#1928);
#1524=LINE('',#8666,#1929);
#1525=LINE('',#8669,#1930);
#1526=LINE('',#8671,#1931);
#1527=LINE('',#8672,#1932);
#1528=LINE('',#8675,#1933);
#1529=LINE('',#8677,#1934);
#1530=LINE('',#8678,#1935);
#1531=LINE('',#8680,#1936);
#1532=LINE('',#8681,#1937);
#1533=LINE('',#8689,#1938);
#1534=LINE('',#8695,#1939);
#1535=LINE('',#8700,#1940);
#1536=LINE('',#8702,#1941);
#1537=LINE('',#8704,#1942);
#1538=LINE('',#8705,#1943);
#1539=LINE('',#8709,#1944);
#1540=LINE('',#8710,#1945);
#1541=LINE('',#8711,#1946);
#1542=LINE('',#8714,#1947);
#1543=LINE('',#8716,#1948);
#1544=LINE('',#8717,#1949);
#1545=LINE('',#8720,#1950);
#1546=LINE('',#8722,#1951);
#1547=LINE('',#8723,#1952);
#1548=LINE('',#8726,#1953);
#1549=LINE('',#8728,#1954);
#1550=LINE('',#8729,#1955);
#1551=LINE('',#8731,#1956);
#1552=LINE('',#8733,#1957);
#1553=LINE('',#8739,#1958);
#1554=LINE('',#8741,#1959);
#1555=LINE('',#8743,#1960);
#1556=LINE('',#8744,#1961);
#1557=LINE('',#8747,#1962);
#1558=LINE('',#8749,#1963);
#1559=LINE('',#8750,#1964);
#1560=LINE('',#8753,#1965);
#1561=LINE('',#8755,#1966);
#1562=LINE('',#8756,#1967);
#1563=LINE('',#8759,#1968);
#1564=LINE('',#8761,#1969);
#1565=LINE('',#8762,#1970);
#1566=LINE('',#8765,#1971);
#1567=LINE('',#8767,#1972);
#1568=LINE('',#8768,#1973);
#1569=LINE('',#8771,#1974);
#1570=LINE('',#8773,#1975);
#1571=LINE('',#8774,#1976);
#1572=LINE('',#8777,#1977);
#1573=LINE('',#8779,#1978);
#1574=LINE('',#8780,#1979);
#1575=LINE('',#8783,#1980);
#1576=LINE('',#8785,#1981);
#1577=LINE('',#8786,#1982);
#1578=LINE('',#8789,#1983);
#1579=LINE('',#8791,#1984);
#1580=LINE('',#8792,#1985);
#1581=LINE('',#8796,#1986);
#1582=LINE('',#8798,#1987);
#1583=LINE('',#8800,#1988);
#1584=LINE('',#8801,#1989);
#1585=LINE('',#8804,#1990);
#1586=LINE('',#8806,#1991);
#1587=LINE('',#8807,#1992);
#1588=LINE('',#8810,#1993);
#1589=LINE('',#8812,#1994);
#1590=LINE('',#8813,#1995);
#1591=LINE('',#8816,#1996);
#1592=LINE('',#8818,#1997);
#1593=LINE('',#8819,#1998);
#1594=LINE('',#8822,#1999);
#1595=LINE('',#8824,#2000);
#1596=LINE('',#8825,#2001);
#1597=LINE('',#8828,#2002);
#1598=LINE('',#8830,#2003);
#1599=LINE('',#8831,#2004);
#1600=LINE('',#8834,#2005);
#1601=LINE('',#8836,#2006);
#1602=LINE('',#8837,#2007);
#1603=LINE('',#8840,#2008);
#1604=LINE('',#8842,#2009);
#1605=LINE('',#8843,#2010);
#1606=LINE('',#8846,#2011);
#1607=LINE('',#8848,#2012);
#1608=LINE('',#8849,#2013);
#1609=LINE('',#8853,#2014);
#1610=LINE('',#8855,#2015);
#1611=LINE('',#8857,#2016);
#1612=LINE('',#8858,#2017);
#1613=LINE('',#8861,#2018);
#1614=LINE('',#8863,#2019);
#1615=LINE('',#8864,#2020);
#1616=LINE('',#8867,#2021);
#1617=LINE('',#8869,#2022);
#1618=LINE('',#8870,#2023);
#1619=LINE('',#8873,#2024);
#1620=LINE('',#8875,#2025);
#1621=LINE('',#8876,#2026);
#1622=LINE('',#8879,#2027);
#1623=LINE('',#8881,#2028);
#1624=LINE('',#8882,#2029);
#1625=LINE('',#8885,#2030);
#1626=LINE('',#8887,#2031);
#1627=LINE('',#8888,#2032);
#1628=LINE('',#8891,#2033);
#1629=LINE('',#8893,#2034);
#1630=LINE('',#8894,#2035);
#1631=LINE('',#8897,#2036);
#1632=LINE('',#8899,#2037);
#1633=LINE('',#8900,#2038);
#1634=LINE('',#8903,#2039);
#1635=LINE('',#8905,#2040);
#1636=LINE('',#8906,#2041);
#1637=LINE('',#8910,#2042);
#1638=LINE('',#8912,#2043);
#1639=LINE('',#8914,#2044);
#1640=LINE('',#8915,#2045);
#1641=LINE('',#8918,#2046);
#1642=LINE('',#8920,#2047);
#1643=LINE('',#8921,#2048);
#1644=LINE('',#8924,#2049);
#1645=LINE('',#8926,#2050);
#1646=LINE('',#8927,#2051);
#1647=LINE('',#8930,#2052);
#1648=LINE('',#8932,#2053);
#1649=LINE('',#8933,#2054);
#1650=LINE('',#8936,#2055);
#1651=LINE('',#8938,#2056);
#1652=LINE('',#8939,#2057);
#1653=LINE('',#8942,#2058);
#1654=LINE('',#8944,#2059);
#1655=LINE('',#8945,#2060);
#1656=LINE('',#8948,#2061);
#1657=LINE('',#8950,#2062);
#1658=LINE('',#8951,#2063);
#1659=LINE('',#8954,#2064);
#1660=LINE('',#8956,#2065);
#1661=LINE('',#8957,#2066);
#1662=LINE('',#8960,#2067);
#1663=LINE('',#8962,#2068);
#1664=LINE('',#8963,#2069);
#1665=LINE('',#8968,#2070);
#1666=LINE('',#8972,#2071);
#1667=LINE('',#8974,#2072);
#1668=LINE('',#8975,#2073);
#1669=LINE('',#8978,#2074);
#1670=LINE('',#8980,#2075);
#1671=LINE('',#8981,#2076);
#1672=LINE('',#8983,#2077);
#1673=LINE('',#8984,#2078);
#1674=LINE('',#8987,#2079);
#1675=LINE('',#8989,#2080);
#1676=LINE('',#8990,#2081);
#1677=LINE('',#8992,#2082);
#1678=LINE('',#8993,#2083);
#1679=LINE('',#8996,#2084);
#1680=LINE('',#8998,#2085);
#1681=LINE('',#8999,#2086);
#1682=LINE('',#9001,#2087);
#1683=LINE('',#9002,#2088);
#1684=LINE('',#9004,#2089);
#1685=LINE('',#9005,#2090);
#1686=LINE('',#9012,#2091);
#1687=LINE('',#9014,#2092);
#1688=LINE('',#9016,#2093);
#1689=LINE('',#9018,#2094);
#1690=LINE('',#9021,#2095);
#1691=LINE('',#9026,#2096);
#1692=LINE('',#9035,#2097);
#1693=LINE('',#9036,#2098);
#1694=LINE('',#9039,#2099);
#1695=LINE('',#9040,#2100);
#1696=LINE('',#9043,#2101);
#1697=LINE('',#9045,#2102);
#1698=LINE('',#9046,#2103);
#1699=LINE('',#9049,#2104);
#1700=LINE('',#9051,#2105);
#1701=LINE('',#9052,#2106);
#1702=LINE('',#9055,#2107);
#1703=LINE('',#9056,#2108);
#1704=LINE('',#9059,#2109);
#1705=LINE('',#9060,#2110);
#1706=LINE('',#9062,#2111);
#1707=LINE('',#9069,#2112);
#1708=LINE('',#9073,#2113);
#1709=LINE('',#9080,#2114);
#1710=LINE('',#9087,#2115);
#1711=LINE('',#9089,#2116);
#1712=LINE('',#9091,#2117);
#1713=LINE('',#9092,#2118);
#1714=LINE('',#9095,#2119);
#1715=LINE('',#9097,#2120);
#1716=LINE('',#9098,#2121);
#1717=LINE('',#9101,#2122);
#1718=LINE('',#9103,#2123);
#1719=LINE('',#9104,#2124);
#1720=LINE('',#9107,#2125);
#1721=LINE('',#9109,#2126);
#1722=LINE('',#9110,#2127);
#1723=LINE('',#9113,#2128);
#1724=LINE('',#9115,#2129);
#1725=LINE('',#9116,#2130);
#1726=LINE('',#9118,#2131);
#1727=LINE('',#9119,#2132);
#1728=LINE('',#9131,#2133);
#1729=LINE('',#9135,#2134);
#1730=LINE('',#9139,#2135);
#1731=LINE('',#9146,#2136);
#1732=LINE('',#9148,#2137);
#1733=LINE('',#9154,#2138);
#1734=LINE('',#9159,#2139);
#1735=LINE('',#9165,#2140);
#1736=LINE('',#9191,#2141);
#1737=LINE('',#9193,#2142);
#1738=LINE('',#9194,#2143);
#1739=LINE('',#9197,#2144);
#1740=LINE('',#9198,#2145);
#1741=LINE('',#9201,#2146);
#1742=LINE('',#9202,#2147);
#1743=LINE('',#9205,#2148);
#1744=LINE('',#9206,#2149);
#1745=LINE('',#9209,#2150);
#1746=LINE('',#9210,#2151);
#1747=LINE('',#9212,#2152);
#1748=LINE('',#9227,#2153);
#1749=LINE('',#9248,#2154);
#1750=LINE('',#9273,#2155);
#1751=LINE('',#9274,#2156);
#1752=LINE('',#9276,#2157);
#1753=LINE('',#9278,#2158);
#1754=LINE('',#9283,#2159);
#1755=LINE('',#9286,#2160);
#1756=LINE('',#9288,#2161);
#1757=LINE('',#9298,#2162);
#1758=LINE('',#9304,#2163);
#1759=LINE('',#9310,#2164);
#1760=LINE('',#9316,#2165);
#1761=LINE('',#9322,#2166);
#1762=LINE('',#9329,#2167);
#1763=LINE('',#9335,#2168);
#1764=LINE('',#9344,#2169);
#1765=LINE('',#9350,#2170);
#1766=LINE('',#9356,#2171);
#1767=LINE('',#9362,#2172);
#1768=LINE('',#9368,#2173);
#1769=LINE('',#9376,#2174);
#1770=LINE('',#9381,#2175);
#1771=LINE('',#9390,#2176);
#1772=LINE('',#9396,#2177);
#1773=LINE('',#9405,#2178);
#1774=LINE('',#9411,#2179);
#1775=LINE('',#9417,#2180);
#1776=LINE('',#9423,#2181);
#1777=LINE('',#9429,#2182);
#1778=LINE('',#9435,#2183);
#1779=LINE('',#9446,#2184);
#1780=LINE('',#9450,#2185);
#1781=LINE('',#9454,#2186);
#1782=LINE('',#9461,#2187);
#1783=LINE('',#9465,#2188);
#1784=LINE('',#9469,#2189);
#1785=LINE('',#9474,#2190);
#1786=LINE('',#9476,#2191);
#1787=LINE('',#9478,#2192);
#1788=LINE('',#9479,#2193);
#1789=LINE('',#9482,#2194);
#1790=LINE('',#9484,#2195);
#1791=LINE('',#9485,#2196);
#1792=LINE('',#9488,#2197);
#1793=LINE('',#9490,#2198);
#1794=LINE('',#9491,#2199);
#1795=LINE('',#9494,#2200);
#1796=LINE('',#9496,#2201);
#1797=LINE('',#9497,#2202);
#1798=LINE('',#9500,#2203);
#1799=LINE('',#9502,#2204);
#1800=LINE('',#9503,#2205);
#1801=LINE('',#9505,#2206);
#1802=LINE('',#9506,#2207);
#1803=VECTOR('',#6117,0.165);
#1804=VECTOR('',#6126,0.165);
#1805=VECTOR('',#6145,0.6);
#1806=VECTOR('',#6148,0.5);
#1807=VECTOR('',#6155,0.5);
#1808=VECTOR('',#6166,0.505);
#1809=VECTOR('',#6173,0.8);
#1810=VECTOR('',#6186,0.505);
#1811=VECTOR('',#6193,0.8);
#1812=VECTOR('',#6206,0.225);
#1813=VECTOR('',#6213,1.1);
#1814=VECTOR('',#6226,0.605);
#1815=VECTOR('',#6233,1.);
#1816=VECTOR('',#6258,0.976185);
#1817=VECTOR('',#6265,0.5);
#1818=VECTOR('',#6270,0.53);
#1819=VECTOR('',#6279,0.976185);
#1820=VECTOR('',#6286,0.53);
#1821=VECTOR('',#6305,1.023815);
#1822=VECTOR('',#6316,1.47);
#1823=VECTOR('',#6321,1.5);
#1824=VECTOR('',#6326,1.47);
#1825=VECTOR('',#6331,1.023815);
#1826=VECTOR('',#6382,1.019052);
#1827=VECTOR('',#6459,0.980948);
#1828=VECTOR('',#6488,1.013815);
#1829=VECTOR('',#6495,0.991185);
#1830=VECTOR('',#6506,1.013815);
#1831=VECTOR('',#6513,0.991185);
#1832=VECTOR('',#6528,1.);
#1833=VECTOR('',#6531,1.);
#1834=VECTOR('',#6536,1.);
#1835=VECTOR('',#6539,1.);
#1836=VECTOR('',#6544,1.);
#1837=VECTOR('',#6545,1.);
#1838=VECTOR('',#6546,1.);
#1839=VECTOR('',#6549,1.);
#1840=VECTOR('',#6550,1.);
#1841=VECTOR('',#6551,1.);
#1842=VECTOR('',#6556,1.);
#1843=VECTOR('',#6557,1.);
#1844=VECTOR('',#6560,1.);
#1845=VECTOR('',#6565,1.);
#1846=VECTOR('',#6566,1.);
#1847=VECTOR('',#6569,1.);
#1848=VECTOR('',#6570,1.);
#1849=VECTOR('',#6577,0.275);
#1850=VECTOR('',#6582,1.);
#1851=VECTOR('',#6585,1.);
#1852=VECTOR('',#6594,1.);
#1853=VECTOR('',#6595,1.);
#1854=VECTOR('',#6596,1.);
#1855=VECTOR('',#6599,1.);
#1856=VECTOR('',#6600,1.);
#1857=VECTOR('',#6603,1.);
#1858=VECTOR('',#6604,1.);
#1859=VECTOR('',#6609,0.275);
#1860=VECTOR('',#6614,0.505);
#1861=VECTOR('',#6617,1.);
#1862=VECTOR('',#6620,1.);
#1863=VECTOR('',#6623,1.);
#1864=VECTOR('',#6624,1.);
#1865=VECTOR('',#6625,1.);
#1866=VECTOR('',#6626,1.);
#1867=VECTOR('',#6629,1.);
#1868=VECTOR('',#6630,1.);
#1869=VECTOR('',#6631,1.);
#1870=VECTOR('',#6634,1.);
#1871=VECTOR('',#6635,1.);
#1872=VECTOR('',#6636,1.);
#1873=VECTOR('',#6639,1.);
#1874=VECTOR('',#6640,1.);
#1875=VECTOR('',#6651,0.275);
#1876=VECTOR('',#6658,0.34);
#1877=VECTOR('',#6663,1.);
#1878=VECTOR('',#6664,1.);
#1879=VECTOR('',#6665,1.);
#1880=VECTOR('',#6666,1.);
#1881=VECTOR('',#6669,1.);
#1882=VECTOR('',#6670,1.);
#1883=VECTOR('',#6671,1.);
#1884=VECTOR('',#6674,1.);
#1885=VECTOR('',#6675,1.);
#1886=VECTOR('',#6676,1.);
#1887=VECTOR('',#6679,1.);
#1888=VECTOR('',#6680,1.);
#1889=VECTOR('',#6681,1.);
#1890=VECTOR('',#6684,1.);
#1891=VECTOR('',#6685,1.);
#1892=VECTOR('',#6686,1.);
#1893=VECTOR('',#6689,1.);
#1894=VECTOR('',#6692,1.);
#1895=VECTOR('',#6699,1.);
#1896=VECTOR('',#6702,1.);
#1897=VECTOR('',#6707,1.);
#1898=VECTOR('',#6710,1.);
#1899=VECTOR('',#6715,1.);
#1900=VECTOR('',#6716,1.);
#1901=VECTOR('',#6717,1.);
#1902=VECTOR('',#6720,1.);
#1903=VECTOR('',#6721,1.);
#1904=VECTOR('',#6722,1.);
#1905=VECTOR('',#6727,1.);
#1906=VECTOR('',#6728,1.);
#1907=VECTOR('',#6731,1.);
#1908=VECTOR('',#6736,1.);
#1909=VECTOR('',#6737,1.);
#1910=VECTOR('',#6740,1.);
#1911=VECTOR('',#6741,1.);
#1912=VECTOR('',#6748,0.275);
#1913=VECTOR('',#6753,1.);
#1914=VECTOR('',#6756,1.);
#1915=VECTOR('',#6765,1.);
#1916=VECTOR('',#6766,1.);
#1917=VECTOR('',#6767,1.);
#1918=VECTOR('',#6770,1.);
#1919=VECTOR('',#6771,1.);
#1920=VECTOR('',#6774,1.);
#1921=VECTOR('',#6775,1.);
#1922=VECTOR('',#6780,0.275);
#1923=VECTOR('',#6785,0.505);
#1924=VECTOR('',#6788,1.);
#1925=VECTOR('',#6791,1.);
#1926=VECTOR('',#6794,1.);
#1927=VECTOR('',#6795,1.);
#1928=VECTOR('',#6796,1.);
#1929=VECTOR('',#6797,1.);
#1930=VECTOR('',#6800,1.);
#1931=VECTOR('',#6801,1.);
#1932=VECTOR('',#6802,1.);
#1933=VECTOR('',#6805,1.);
#1934=VECTOR('',#6806,1.);
#1935=VECTOR('',#6807,1.);
#1936=VECTOR('',#6810,1.);
#1937=VECTOR('',#6811,1.);
#1938=VECTOR('',#6822,0.275);
#1939=VECTOR('',#6829,0.34);
#1940=VECTOR('',#6834,1.);
#1941=VECTOR('',#6835,1.);
#1942=VECTOR('',#6836,1.);
#1943=VECTOR('',#6837,1.);
#1944=VECTOR('',#6840,1.);
#1945=VECTOR('',#6841,1.);
#1946=VECTOR('',#6842,1.);
#1947=VECTOR('',#6845,1.);
#1948=VECTOR('',#6846,1.);
#1949=VECTOR('',#6847,1.);
#1950=VECTOR('',#6850,1.);
#1951=VECTOR('',#6851,1.);
#1952=VECTOR('',#6852,1.);
#1953=VECTOR('',#6855,1.);
#1954=VECTOR('',#6856,1.);
#1955=VECTOR('',#6857,1.);
#1956=VECTOR('',#6860,1.);
#1957=VECTOR('',#6863,1.);
#1958=VECTOR('',#6870,1.);
#1959=VECTOR('',#6871,1.);
#1960=VECTOR('',#6872,1.);
#1961=VECTOR('',#6873,1.);
#1962=VECTOR('',#6876,1.);
#1963=VECTOR('',#6877,1.);
#1964=VECTOR('',#6878,1.);
#1965=VECTOR('',#6881,1.);
#1966=VECTOR('',#6882,1.);
#1967=VECTOR('',#6883,1.);
#1968=VECTOR('',#6886,1.);
#1969=VECTOR('',#6887,1.);
#1970=VECTOR('',#6888,1.);
#1971=VECTOR('',#6891,1.);
#1972=VECTOR('',#6892,1.);
#1973=VECTOR('',#6893,1.);
#1974=VECTOR('',#6896,1.);
#1975=VECTOR('',#6897,1.);
#1976=VECTOR('',#6898,1.);
#1977=VECTOR('',#6901,1.);
#1978=VECTOR('',#6902,1.);
#1979=VECTOR('',#6903,1.);
#1980=VECTOR('',#6906,1.);
#1981=VECTOR('',#6907,1.);
#1982=VECTOR('',#6908,1.);
#1983=VECTOR('',#6911,1.);
#1984=VECTOR('',#6912,1.);
#1985=VECTOR('',#6913,1.);
#1986=VECTOR('',#6916,1.);
#1987=VECTOR('',#6917,1.);
#1988=VECTOR('',#6918,1.);
#1989=VECTOR('',#6919,1.);
#1990=VECTOR('',#6922,1.);
#1991=VECTOR('',#6923,1.);
#1992=VECTOR('',#6924,1.);
#1993=VECTOR('',#6927,1.);
#1994=VECTOR('',#6928,1.);
#1995=VECTOR('',#6929,1.);
#1996=VECTOR('',#6932,1.);
#1997=VECTOR('',#6933,1.);
#1998=VECTOR('',#6934,1.);
#1999=VECTOR('',#6937,1.);
#2000=VECTOR('',#6938,1.);
#2001=VECTOR('',#6939,1.);
#2002=VECTOR('',#6942,1.);
#2003=VECTOR('',#6943,1.);
#2004=VECTOR('',#6944,1.);
#2005=VECTOR('',#6947,1.);
#2006=VECTOR('',#6948,1.);
#2007=VECTOR('',#6949,1.);
#2008=VECTOR('',#6952,1.);
#2009=VECTOR('',#6953,1.);
#2010=VECTOR('',#6954,1.);
#2011=VECTOR('',#6957,1.);
#2012=VECTOR('',#6958,1.);
#2013=VECTOR('',#6959,1.);
#2014=VECTOR('',#6962,1.);
#2015=VECTOR('',#6963,1.);
#2016=VECTOR('',#6964,1.);
#2017=VECTOR('',#6965,1.);
#2018=VECTOR('',#6968,1.);
#2019=VECTOR('',#6969,1.);
#2020=VECTOR('',#6970,1.);
#2021=VECTOR('',#6973,1.);
#2022=VECTOR('',#6974,1.);
#2023=VECTOR('',#6975,1.);
#2024=VECTOR('',#6978,1.);
#2025=VECTOR('',#6979,1.);
#2026=VECTOR('',#6980,1.);
#2027=VECTOR('',#6983,1.);
#2028=VECTOR('',#6984,1.);
#2029=VECTOR('',#6985,1.);
#2030=VECTOR('',#6988,1.);
#2031=VECTOR('',#6989,1.);
#2032=VECTOR('',#6990,1.);
#2033=VECTOR('',#6993,1.);
#2034=VECTOR('',#6994,1.);
#2035=VECTOR('',#6995,1.);
#2036=VECTOR('',#6998,1.);
#2037=VECTOR('',#6999,1.);
#2038=VECTOR('',#7000,1.);
#2039=VECTOR('',#7003,1.);
#2040=VECTOR('',#7004,1.);
#2041=VECTOR('',#7005,1.);
#2042=VECTOR('',#7008,1.);
#2043=VECTOR('',#7009,1.);
#2044=VECTOR('',#7010,1.);
#2045=VECTOR('',#7011,1.);
#2046=VECTOR('',#7014,1.);
#2047=VECTOR('',#7015,1.);
#2048=VECTOR('',#7016,1.);
#2049=VECTOR('',#7019,1.);
#2050=VECTOR('',#7020,1.);
#2051=VECTOR('',#7021,1.);
#2052=VECTOR('',#7024,1.);
#2053=VECTOR('',#7025,1.);
#2054=VECTOR('',#7026,1.);
#2055=VECTOR('',#7029,1.);
#2056=VECTOR('',#7030,1.);
#2057=VECTOR('',#7031,1.);
#2058=VECTOR('',#7034,1.);
#2059=VECTOR('',#7035,1.);
#2060=VECTOR('',#7036,1.);
#2061=VECTOR('',#7039,1.);
#2062=VECTOR('',#7040,1.);
#2063=VECTOR('',#7041,1.);
#2064=VECTOR('',#7044,1.);
#2065=VECTOR('',#7045,1.);
#2066=VECTOR('',#7046,1.);
#2067=VECTOR('',#7049,1.);
#2068=VECTOR('',#7050,1.);
#2069=VECTOR('',#7051,1.);
#2070=VECTOR('',#7056,0.21);
#2071=VECTOR('',#7061,1.);
#2072=VECTOR('',#7062,1.);
#2073=VECTOR('',#7063,1.);
#2074=VECTOR('',#7066,1.);
#2075=VECTOR('',#7067,1.);
#2076=VECTOR('',#7068,1.);
#2077=VECTOR('',#7071,1.);
#2078=VECTOR('',#7072,1.);
#2079=VECTOR('',#7075,1.);
#2080=VECTOR('',#7076,1.);
#2081=VECTOR('',#7077,1.);
#2082=VECTOR('',#7080,1.);
#2083=VECTOR('',#7081,1.);
#2084=VECTOR('',#7084,1.);
#2085=VECTOR('',#7085,1.);
#2086=VECTOR('',#7086,1.);
#2087=VECTOR('',#7089,1.);
#2088=VECTOR('',#7090,1.);
#2089=VECTOR('',#7093,1.);
#2090=VECTOR('',#7094,1.);
#2091=VECTOR('',#7103,1.);
#2092=VECTOR('',#7104,1.);
#2093=VECTOR('',#7105,1.);
#2094=VECTOR('',#7106,1.);
#2095=VECTOR('',#7109,1.);
#2096=VECTOR('',#7114,0.21);
#2097=VECTOR('',#7125,1.);
#2098=VECTOR('',#7126,1.);
#2099=VECTOR('',#7129,1.);
#2100=VECTOR('',#7130,1.);
#2101=VECTOR('',#7133,1.);
#2102=VECTOR('',#7134,1.);
#2103=VECTOR('',#7135,1.);
#2104=VECTOR('',#7138,1.);
#2105=VECTOR('',#7139,1.);
#2106=VECTOR('',#7140,1.);
#2107=VECTOR('',#7143,1.);
#2108=VECTOR('',#7144,1.);
#2109=VECTOR('',#7147,1.);
#2110=VECTOR('',#7148,1.);
#2111=VECTOR('',#7151,1.);
#2112=VECTOR('',#7160,0.275);
#2113=VECTOR('',#7165,0.265);
#2114=VECTOR('',#7174,0.5);
#2115=VECTOR('',#7183,1.);
#2116=VECTOR('',#7184,1.);
#2117=VECTOR('',#7185,1.);
#2118=VECTOR('',#7186,1.);
#2119=VECTOR('',#7189,1.);
#2120=VECTOR('',#7190,1.);
#2121=VECTOR('',#7191,1.);
#2122=VECTOR('',#7194,1.);
#2123=VECTOR('',#7195,1.);
#2124=VECTOR('',#7196,1.);
#2125=VECTOR('',#7199,1.);
#2126=VECTOR('',#7200,1.);
#2127=VECTOR('',#7201,1.);
#2128=VECTOR('',#7204,1.);
#2129=VECTOR('',#7205,1.);
#2130=VECTOR('',#7206,1.);
#2131=VECTOR('',#7209,1.);
#2132=VECTOR('',#7210,1.);
#2133=VECTOR('',#7227,0.4);
#2134=VECTOR('',#7232,0.425);
#2135=VECTOR('',#7237,0.41);
#2136=VECTOR('',#7246,0.26);
#2137=VECTOR('',#7249,0.25);
#2138=VECTOR('',#7256,0.4);
#2139=VECTOR('',#7263,0.36);
#2140=VECTOR('',#7270,0.734027674973257);
#2141=VECTOR('',#7273,1.);
#2142=VECTOR('',#7274,1.);
#2143=VECTOR('',#7275,1.);
#2144=VECTOR('',#7278,1.);
#2145=VECTOR('',#7279,1.);
#2146=VECTOR('',#7282,1.);
#2147=VECTOR('',#7283,1.);
#2148=VECTOR('',#7286,1.);
#2149=VECTOR('',#7287,1.);
#2150=VECTOR('',#7290,1.);
#2151=VECTOR('',#7291,1.);
#2152=VECTOR('',#7294,1.);
#2153=VECTOR('',#7303,0.734027674973257);
#2154=VECTOR('',#7310,0.734027674973257);
#2155=VECTOR('',#7313,1.);
#2156=VECTOR('',#7314,1.);
#2157=VECTOR('',#7317,1.);
#2158=VECTOR('',#7320,1.);
#2159=VECTOR('',#7325,0.4);
#2160=VECTOR('',#7330,1.);
#2161=VECTOR('',#7333,1.);
#2162=VECTOR('',#7348,0.165);
#2163=VECTOR('',#7355,0.165);
#2164=VECTOR('',#7362,0.165);
#2165=VECTOR('',#7369,0.165);
#2166=VECTOR('',#7376,1.2);
#2167=VECTOR('',#7385,1.5);
#2168=VECTOR('',#7392,2.2);
#2169=VECTOR('',#7405,0.165);
#2170=VECTOR('',#7412,0.165);
#2171=VECTOR('',#7419,0.165);
#2172=VECTOR('',#7426,0.165);
#2173=VECTOR('',#7433,1.2);
#2174=VECTOR('',#7444,1.5);
#2175=VECTOR('',#7449,2.2);
#2176=VECTOR('',#7462,2.2);
#2177=VECTOR('',#7469,2.5);
#2178=VECTOR('',#7482,0.225);
#2179=VECTOR('',#7489,0.225);
#2180=VECTOR('',#7496,0.225);
#2181=VECTOR('',#7503,0.225);
#2182=VECTOR('',#7510,1.2);
#2183=VECTOR('',#7517,2.5);
#2184=VECTOR('',#7534,0.325);
#2185=VECTOR('',#7539,0.35);
#2186=VECTOR('',#7544,0.335);
#2187=VECTOR('',#7553,0.21);
#2188=VECTOR('',#7558,0.2);
#2189=VECTOR('',#7563,0.18);
#2190=VECTOR('',#7568,1.);
#2191=VECTOR('',#7569,1.);
#2192=VECTOR('',#7570,1.);
#2193=VECTOR('',#7571,1.);
#2194=VECTOR('',#7574,1.);
#2195=VECTOR('',#7575,1.);
#2196=VECTOR('',#7576,1.);
#2197=VECTOR('',#7579,1.);
#2198=VECTOR('',#7580,1.);
#2199=VECTOR('',#7581,1.);
#2200=VECTOR('',#7584,1.);
#2201=VECTOR('',#7585,1.);
#2202=VECTOR('',#7586,1.);
#2203=VECTOR('',#7589,1.);
#2204=VECTOR('',#7590,1.);
#2205=VECTOR('',#7591,1.);
#2206=VECTOR('',#7594,1.);
#2207=VECTOR('',#7595,1.);
#2208=CIRCLE('',#5513,0.165);
#2209=CIRCLE('',#5514,0.165);
#2210=CIRCLE('',#5517,0.165);
#2211=CIRCLE('',#5518,0.165);
#2212=CIRCLE('',#5521,0.6);
#2213=CIRCLE('',#5522,0.5);
#2214=CIRCLE('',#5524,0.6);
#2215=CIRCLE('',#5525,0.5);
#2216=CIRCLE('',#5528,0.5);
#2217=CIRCLE('',#5530,0.5);
#2218=CIRCLE('',#5535,0.505);
#2219=CIRCLE('',#5536,0.505);
#2220=CIRCLE('',#5538,0.8);
#2221=CIRCLE('',#5539,0.8);
#2222=CIRCLE('',#5544,0.505);
#2223=CIRCLE('',#5545,0.505);
#2224=CIRCLE('',#5547,0.8);
#2225=CIRCLE('',#5548,0.8);
#2226=CIRCLE('',#5553,0.225);
#2227=CIRCLE('',#5554,0.225);
#2228=CIRCLE('',#5556,1.1);
#2229=CIRCLE('',#5557,1.1);
#2230=CIRCLE('',#5562,0.605);
#2231=CIRCLE('',#5563,0.605);
#2232=CIRCLE('',#5565,1.);
#2233=CIRCLE('',#5566,1.);
#2234=CIRCLE('',#5572,0.976185);
#2235=CIRCLE('',#5573,0.976185);
#2236=CIRCLE('',#5574,0.247676);
#2237=CIRCLE('',#5575,0.976185);
#2238=CIRCLE('',#5576,0.976185);
#2239=CIRCLE('',#5578,0.976185);
#2240=CIRCLE('',#5580,0.5);
#2241=CIRCLE('',#5581,0.5);
#2242=CIRCLE('',#5583,0.56);
#2243=CIRCLE('',#5586,0.976185);
#2244=CIRCLE('',#5588,0.56);
#2245=CIRCLE('',#5592,1.023815);
#2246=CIRCLE('',#5593,1.023815);
#2247=CIRCLE('',#5594,0.247676);
#2248=CIRCLE('',#5595,1.023815);
#2249=CIRCLE('',#5596,1.023815);
#2250=CIRCLE('',#5598,1.023815);
#2251=CIRCLE('',#5600,1.44);
#2252=CIRCLE('',#5601,1.023815);
#2253=CIRCLE('',#5603,1.5);
#2254=CIRCLE('',#5605,1.5);
#2255=CIRCLE('',#5607,1.44);
#2256=CIRCLE('',#5612,0.23815);
#2257=CIRCLE('',#5614,0.23815);
#2258=CIRCLE('',#5616,0.23815);
#2259=CIRCLE('',#5618,0.23815);
#2260=CIRCLE('',#5620,0.23815);
#2261=CIRCLE('',#5622,0.23815);
#2262=CIRCLE('',#5624,0.23815);
#2263=CIRCLE('',#5626,0.23815);
#2264=CIRCLE('',#5629,0.243053047864041);
#2265=CIRCLE('',#5630,0.243053047864041);
#2266=CIRCLE('',#5632,1.019052);
#2267=CIRCLE('',#5633,1.019052);
#2268=CIRCLE('',#5634,1.019052);
#2269=CIRCLE('',#5635,1.019052);
#2270=CIRCLE('',#5636,1.019052);
#2271=CIRCLE('',#5637,1.019052);
#2272=CIRCLE('',#5638,1.019052);
#2273=CIRCLE('',#5639,1.019052);
#2274=CIRCLE('',#5640,1.019052);
#2275=CIRCLE('',#5642,0.980948);
#2276=CIRCLE('',#5643,0.243053047864041);
#2277=CIRCLE('',#5645,0.243053047864041);
#2278=CIRCLE('',#5647,0.980948);
#2279=CIRCLE('',#5648,0.243053047864041);
#2280=CIRCLE('',#5650,0.243053047864041);
#2281=CIRCLE('',#5652,0.980948);
#2282=CIRCLE('',#5653,0.243053047864041);
#2283=CIRCLE('',#5655,0.243053047864041);
#2284=CIRCLE('',#5657,0.980948);
#2285=CIRCLE('',#5658,0.243053047864041);
#2286=CIRCLE('',#5660,0.243053047864041);
#2287=CIRCLE('',#5662,0.980948);
#2288=CIRCLE('',#5663,0.243053047864041);
#2289=CIRCLE('',#5665,0.243053047864041);
#2290=CIRCLE('',#5667,0.980948);
#2291=CIRCLE('',#5668,0.243053047864041);
#2292=CIRCLE('',#5670,0.243053047864041);
#2293=CIRCLE('',#5672,0.980948);
#2294=CIRCLE('',#5673,0.980948);
#2295=CIRCLE('',#5674,0.980948);
#2296=CIRCLE('',#5676,0.243053047864041);
#2297=CIRCLE('',#5678,0.243053047864041);
#2298=CIRCLE('',#5683,1.013815);
#2299=CIRCLE('',#5684,0.991185);
#2300=CIRCLE('',#5686,1.013815);
#2301=CIRCLE('',#5688,0.991185);
#2302=CIRCLE('',#5691,1.013815);
#2303=CIRCLE('',#5692,0.991185);
#2304=CIRCLE('',#5694,1.013815);
#2305=CIRCLE('',#5696,0.991185);
#2306=CIRCLE('',#5705,0.525);
#2307=CIRCLE('',#5706,0.525);
#2308=CIRCLE('',#5708,0.525);
#2309=CIRCLE('',#5709,0.525);
#2310=CIRCLE('',#5712,0.505);
#2311=CIRCLE('',#5715,0.525);
#2312=CIRCLE('',#5718,0.505);
#2313=CIRCLE('',#5720,0.275);
#2314=CIRCLE('',#5721,0.275);
#2315=CIRCLE('',#5723,0.525);
#2316=CIRCLE('',#5724,0.525);
#2317=CIRCLE('',#5726,0.525);
#2318=CIRCLE('',#5731,0.275);
#2319=CIRCLE('',#5732,0.275);
#2320=CIRCLE('',#5744,0.275);
#2321=CIRCLE('',#5745,0.275);
#2322=CIRCLE('',#5747,0.34);
#2323=CIRCLE('',#5748,0.34);
#2324=CIRCLE('',#5759,0.525);
#2325=CIRCLE('',#5760,0.525);
#2326=CIRCLE('',#5762,0.525);
#2327=CIRCLE('',#5763,0.525);
#2328=CIRCLE('',#5766,0.505);
#2329=CIRCLE('',#5769,0.525);
#2330=CIRCLE('',#5772,0.505);
#2331=CIRCLE('',#5774,0.275);
#2332=CIRCLE('',#5775,0.275);
#2333=CIRCLE('',#5777,0.525);
#2334=CIRCLE('',#5778,0.525);
#2335=CIRCLE('',#5780,0.525);
#2336=CIRCLE('',#5785,0.275);
#2337=CIRCLE('',#5786,0.275);
#2338=CIRCLE('',#5798,0.275);
#2339=CIRCLE('',#5799,0.275);
#2340=CIRCLE('',#5801,0.34);
#2341=CIRCLE('',#5802,0.34);
#2342=CIRCLE('',#5849,0.21);
#2343=CIRCLE('',#5850,0.21);
#2344=CIRCLE('',#5865,0.2117);
#2345=CIRCLE('',#5866,0.2117);
#2346=CIRCLE('',#5867,0.2117);
#2347=CIRCLE('',#5869,0.2117);
#2348=CIRCLE('',#5880,0.285);
#2349=CIRCLE('',#5881,0.265);
#2350=CIRCLE('',#5883,0.265);
#2351=CIRCLE('',#5885,0.5);
#2352=CIRCLE('',#5887,0.5);
#2353=CIRCLE('',#5899,0.24505);
#2354=CIRCLE('',#5901,0.375);
#2355=CIRCLE('',#5903,0.425);
#2356=CIRCLE('',#5905,0.425);
#2357=CIRCLE('',#5907,0.395);
#2358=CIRCLE('',#5909,0.27);
#2359=CIRCLE('',#5911,0.24505);
#2360=CIRCLE('',#5915,0.3933);
#2361=CIRCLE('',#5916,0.3933);
#2362=CIRCLE('',#5918,0.32);
#2363=CIRCLE('',#5921,0.6175);
#2364=CIRCLE('',#5932,0.6175);
#2365=CIRCLE('',#5934,0.6175);
#2366=CIRCLE('',#5939,0.338975);
#2367=CIRCLE('',#5940,0.338975);
#2368=CIRCLE('',#5949,0.165);
#2369=CIRCLE('',#5950,0.165);
#2370=CIRCLE('',#5952,0.165);
#2371=CIRCLE('',#5953,0.165);
#2372=CIRCLE('',#5955,0.165);
#2373=CIRCLE('',#5956,0.165);
#2374=CIRCLE('',#5958,0.165);
#2375=CIRCLE('',#5959,0.165);
#2376=CIRCLE('',#5961,1.2);
#2377=CIRCLE('',#5962,1.2);
#2378=CIRCLE('',#5964,1.5);
#2379=CIRCLE('',#5966,1.5);
#2380=CIRCLE('',#5968,2.2);
#2381=CIRCLE('',#5969,2.2);
#2382=CIRCLE('',#5974,0.165);
#2383=CIRCLE('',#5975,0.165);
#2384=CIRCLE('',#5977,0.165);
#2385=CIRCLE('',#5978,0.165);
#2386=CIRCLE('',#5980,0.165);
#2387=CIRCLE('',#5981,0.165);
#2388=CIRCLE('',#5983,0.165);
#2389=CIRCLE('',#5984,0.165);
#2390=CIRCLE('',#5986,1.2);
#2391=CIRCLE('',#5987,1.2);
#2392=CIRCLE('',#5989,1.5);
#2393=CIRCLE('',#5991,1.5);
#2394=CIRCLE('',#5993,2.2);
#2395=CIRCLE('',#5994,2.2);
#2396=CIRCLE('',#5999,2.2);
#2397=CIRCLE('',#6000,2.2);
#2398=CIRCLE('',#6002,2.5);
#2399=CIRCLE('',#6003,2.5);
#2400=CIRCLE('',#6008,0.225);
#2401=CIRCLE('',#6009,0.225);
#2402=CIRCLE('',#6011,0.225);
#2403=CIRCLE('',#6012,0.225);
#2404=CIRCLE('',#6014,0.225);
#2405=CIRCLE('',#6015,0.225);
#2406=CIRCLE('',#6017,0.225);
#2407=CIRCLE('',#6018,0.225);
#2408=CIRCLE('',#6020,1.2);
#2409=CIRCLE('',#6021,1.2);
#2410=CIRCLE('',#6023,2.5);
#2411=CIRCLE('',#6024,2.5);
#2412=CIRCLE('',#6029,0.3);
#2413=CIRCLE('',#6031,0.35);
#2414=CIRCLE('',#6033,0.35);
#2415=CIRCLE('',#6035,0.32);
#2416=CIRCLE('',#6037,0.22);
#2417=CIRCLE('',#6039,0.1954);
#2418=CIRCLE('',#6041,0.1954);
#2419=CIRCLE('',#6043,0.16);
#2420=VERTEX_POINT('',#7712);
#2421=VERTEX_POINT('',#7714);
#2422=VERTEX_POINT('',#7719);
#2423=VERTEX_POINT('',#7721);
#2424=VERTEX_POINT('',#7726);
#2425=VERTEX_POINT('',#7728);
#2426=VERTEX_POINT('',#7731);
#2427=VERTEX_POINT('',#7733);
#2428=VERTEX_POINT('',#7738);
#2429=VERTEX_POINT('',#7742);
#2430=VERTEX_POINT('',#7749);
#2431=VERTEX_POINT('',#7751);
#2432=VERTEX_POINT('',#7755);
#2433=VERTEX_POINT('',#7757);
#2434=VERTEX_POINT('',#7764);
#2435=VERTEX_POINT('',#7766);
#2436=VERTEX_POINT('',#7770);
#2437=VERTEX_POINT('',#7772);
#2438=VERTEX_POINT('',#7779);
#2439=VERTEX_POINT('',#7781);
#2440=VERTEX_POINT('',#7785);
#2441=VERTEX_POINT('',#7787);
#2442=VERTEX_POINT('',#7794);
#2443=VERTEX_POINT('',#7796);
#2444=VERTEX_POINT('',#7800);
#2445=VERTEX_POINT('',#7802);
#2446=VERTEX_POINT('',#7810);
#2447=VERTEX_POINT('',#7811);
#2448=VERTEX_POINT('',#7814);
#2449=VERTEX_POINT('',#7816);
#2450=VERTEX_POINT('',#7820);
#2451=VERTEX_POINT('',#7824);
#2452=VERTEX_POINT('',#7826);
#2453=VERTEX_POINT('',#7830);
#2454=VERTEX_POINT('',#7835);
#2455=VERTEX_POINT('',#7839);
#2456=VERTEX_POINT('',#7845);
#2457=VERTEX_POINT('',#7846);
#2458=VERTEX_POINT('',#7849);
#2459=VERTEX_POINT('',#7851);
#2460=VERTEX_POINT('',#7855);
#2461=VERTEX_POINT('',#7859);
#2462=VERTEX_POINT('',#7861);
#2463=VERTEX_POINT('',#7864);
#2464=VERTEX_POINT('',#7868);
#2465=VERTEX_POINT('',#7872);
#2466=VERTEX_POINT('',#7880);
#2467=VERTEX_POINT('',#7881);
#2468=VERTEX_POINT('',#7884);
#2469=VERTEX_POINT('',#7885);
#2470=VERTEX_POINT('',#7888);
#2471=VERTEX_POINT('',#7889);
#2472=VERTEX_POINT('',#7892);
#2473=VERTEX_POINT('',#7893);
#2474=VERTEX_POINT('',#7896);
#2475=VERTEX_POINT('',#7897);
#2476=VERTEX_POINT('',#7900);
#2477=VERTEX_POINT('',#7901);
#2478=VERTEX_POINT('',#7904);
#2479=VERTEX_POINT('',#7905);
#2480=VERTEX_POINT('',#7908);
#2481=VERTEX_POINT('',#7909);
#2482=VERTEX_POINT('',#7913);
#2483=VERTEX_POINT('',#7914);
#2484=VERTEX_POINT('',#7937);
#2485=VERTEX_POINT('',#7939);
#2486=VERTEX_POINT('',#7964);
#2487=VERTEX_POINT('',#7966);
#2488=VERTEX_POINT('',#7989);
#2489=VERTEX_POINT('',#7991);
#2490=VERTEX_POINT('',#8014);
#2491=VERTEX_POINT('',#8016);
#2492=VERTEX_POINT('',#8029);
#2493=VERTEX_POINT('',#8032);
#2494=VERTEX_POINT('',#8045);
#2495=VERTEX_POINT('',#8047);
#2496=VERTEX_POINT('',#8070);
#2497=VERTEX_POINT('',#8072);
#2498=VERTEX_POINT('',#8095);
#2499=VERTEX_POINT('',#8097);
#2500=VERTEX_POINT('',#8120);
#2501=VERTEX_POINT('',#8122);
#2502=VERTEX_POINT('',#8147);
#2503=VERTEX_POINT('',#8151);
#2504=VERTEX_POINT('',#8176);
#2505=VERTEX_POINT('',#8180);
#2506=VERTEX_POINT('',#8205);
#2507=VERTEX_POINT('',#8209);
#2508=VERTEX_POINT('',#8210);
#2509=VERTEX_POINT('',#8237);
#2510=VERTEX_POINT('',#8241);
#2511=VERTEX_POINT('',#8266);
#2512=VERTEX_POINT('',#8270);
#2513=VERTEX_POINT('',#8295);
#2514=VERTEX_POINT('',#8299);
#2515=VERTEX_POINT('',#8324);
#2516=VERTEX_POINT('',#8327);
#2517=VERTEX_POINT('',#8329);
#2518=VERTEX_POINT('',#8361);
#2519=VERTEX_POINT('',#8363);
#2520=VERTEX_POINT('',#8366);
#2521=VERTEX_POINT('',#8370);
#2522=VERTEX_POINT('',#8375);
#2523=VERTEX_POINT('',#8377);
#2524=VERTEX_POINT('',#8380);
#2525=VERTEX_POINT('',#8384);
#2526=VERTEX_POINT('',#8395);
#2527=VERTEX_POINT('',#8396);
#2528=VERTEX_POINT('',#8398);
#2529=VERTEX_POINT('',#8400);
#2530=VERTEX_POINT('',#8404);
#2531=VERTEX_POINT('',#8405);
#2532=VERTEX_POINT('',#8407);
#2533=VERTEX_POINT('',#8409);
#2534=VERTEX_POINT('',#8413);
#2535=VERTEX_POINT('',#8415);
#2536=VERTEX_POINT('',#8419);
#2537=VERTEX_POINT('',#8421);
#2538=VERTEX_POINT('',#8424);
#2539=VERTEX_POINT('',#8427);
#2540=VERTEX_POINT('',#8431);
#2541=VERTEX_POINT('',#8435);
#2542=VERTEX_POINT('',#8439);
#2543=VERTEX_POINT('',#8442);
#2544=VERTEX_POINT('',#8445);
#2545=VERTEX_POINT('',#8447);
#2546=VERTEX_POINT('',#8451);
#2547=VERTEX_POINT('',#8452);
#2548=VERTEX_POINT('',#8454);
#2549=VERTEX_POINT('',#8456);
#2550=VERTEX_POINT('',#8462);
#2551=VERTEX_POINT('',#8464);
#2552=VERTEX_POINT('',#8468);
#2553=VERTEX_POINT('',#8472);
#2554=VERTEX_POINT('',#8476);
#2555=VERTEX_POINT('',#8478);
#2556=VERTEX_POINT('',#8488);
#2557=VERTEX_POINT('',#8489);
#2558=VERTEX_POINT('',#8491);
#2559=VERTEX_POINT('',#8493);
#2560=VERTEX_POINT('',#8497);
#2561=VERTEX_POINT('',#8499);
#2562=VERTEX_POINT('',#8503);
#2563=VERTEX_POINT('',#8505);
#2564=VERTEX_POINT('',#8515);
#2565=VERTEX_POINT('',#8517);
#2566=VERTEX_POINT('',#8521);
#2567=VERTEX_POINT('',#8523);
#2568=VERTEX_POINT('',#8527);
#2569=VERTEX_POINT('',#8528);
#2570=VERTEX_POINT('',#8530);
#2571=VERTEX_POINT('',#8532);
#2572=VERTEX_POINT('',#8536);
#2573=VERTEX_POINT('',#8537);
#2574=VERTEX_POINT('',#8542);
#2575=VERTEX_POINT('',#8544);
#2576=VERTEX_POINT('',#8548);
#2577=VERTEX_POINT('',#8550);
#2578=VERTEX_POINT('',#8554);
#2579=VERTEX_POINT('',#8556);
#2580=VERTEX_POINT('',#8566);
#2581=VERTEX_POINT('',#8567);
#2582=VERTEX_POINT('',#8569);
#2583=VERTEX_POINT('',#8571);
#2584=VERTEX_POINT('',#8575);
#2585=VERTEX_POINT('',#8576);
#2586=VERTEX_POINT('',#8578);
#2587=VERTEX_POINT('',#8580);
#2588=VERTEX_POINT('',#8584);
#2589=VERTEX_POINT('',#8586);
#2590=VERTEX_POINT('',#8590);
#2591=VERTEX_POINT('',#8592);
#2592=VERTEX_POINT('',#8595);
#2593=VERTEX_POINT('',#8598);
#2594=VERTEX_POINT('',#8602);
#2595=VERTEX_POINT('',#8606);
#2596=VERTEX_POINT('',#8610);
#2597=VERTEX_POINT('',#8613);
#2598=VERTEX_POINT('',#8616);
#2599=VERTEX_POINT('',#8618);
#2600=VERTEX_POINT('',#8622);
#2601=VERTEX_POINT('',#8623);
#2602=VERTEX_POINT('',#8625);
#2603=VERTEX_POINT('',#8627);
#2604=VERTEX_POINT('',#8633);
#2605=VERTEX_POINT('',#8635);
#2606=VERTEX_POINT('',#8639);
#2607=VERTEX_POINT('',#8643);
#2608=VERTEX_POINT('',#8647);
#2609=VERTEX_POINT('',#8649);
#2610=VERTEX_POINT('',#8659);
#2611=VERTEX_POINT('',#8660);
#2612=VERTEX_POINT('',#8662);
#2613=VERTEX_POINT('',#8664);
#2614=VERTEX_POINT('',#8668);
#2615=VERTEX_POINT('',#8670);
#2616=VERTEX_POINT('',#8674);
#2617=VERTEX_POINT('',#8676);
#2618=VERTEX_POINT('',#8686);
#2619=VERTEX_POINT('',#8688);
#2620=VERTEX_POINT('',#8692);
#2621=VERTEX_POINT('',#8694);
#2622=VERTEX_POINT('',#8698);
#2623=VERTEX_POINT('',#8699);
#2624=VERTEX_POINT('',#8701);
#2625=VERTEX_POINT('',#8703);
#2626=VERTEX_POINT('',#8707);
#2627=VERTEX_POINT('',#8708);
#2628=VERTEX_POINT('',#8713);
#2629=VERTEX_POINT('',#8715);
#2630=VERTEX_POINT('',#8719);
#2631=VERTEX_POINT('',#8721);
#2632=VERTEX_POINT('',#8725);
#2633=VERTEX_POINT('',#8727);
#2634=VERTEX_POINT('',#8737);
#2635=VERTEX_POINT('',#8738);
#2636=VERTEX_POINT('',#8740);
#2637=VERTEX_POINT('',#8742);
#2638=VERTEX_POINT('',#8746);
#2639=VERTEX_POINT('',#8748);
#2640=VERTEX_POINT('',#8752);
#2641=VERTEX_POINT('',#8754);
#2642=VERTEX_POINT('',#8758);
#2643=VERTEX_POINT('',#8760);
#2644=VERTEX_POINT('',#8764);
#2645=VERTEX_POINT('',#8766);
#2646=VERTEX_POINT('',#8770);
#2647=VERTEX_POINT('',#8772);
#2648=VERTEX_POINT('',#8776);
#2649=VERTEX_POINT('',#8778);
#2650=VERTEX_POINT('',#8782);
#2651=VERTEX_POINT('',#8784);
#2652=VERTEX_POINT('',#8788);
#2653=VERTEX_POINT('',#8790);
#2654=VERTEX_POINT('',#8794);
#2655=VERTEX_POINT('',#8795);
#2656=VERTEX_POINT('',#8797);
#2657=VERTEX_POINT('',#8799);
#2658=VERTEX_POINT('',#8803);
#2659=VERTEX_POINT('',#8805);
#2660=VERTEX_POINT('',#8809);
#2661=VERTEX_POINT('',#8811);
#2662=VERTEX_POINT('',#8815);
#2663=VERTEX_POINT('',#8817);
#2664=VERTEX_POINT('',#8821);
#2665=VERTEX_POINT('',#8823);
#2666=VERTEX_POINT('',#8827);
#2667=VERTEX_POINT('',#8829);
#2668=VERTEX_POINT('',#8833);
#2669=VERTEX_POINT('',#8835);
#2670=VERTEX_POINT('',#8839);
#2671=VERTEX_POINT('',#8841);
#2672=VERTEX_POINT('',#8845);
#2673=VERTEX_POINT('',#8847);
#2674=VERTEX_POINT('',#8851);
#2675=VERTEX_POINT('',#8852);
#2676=VERTEX_POINT('',#8854);
#2677=VERTEX_POINT('',#8856);
#2678=VERTEX_POINT('',#8860);
#2679=VERTEX_POINT('',#8862);
#2680=VERTEX_POINT('',#8866);
#2681=VERTEX_POINT('',#8868);
#2682=VERTEX_POINT('',#8872);
#2683=VERTEX_POINT('',#8874);
#2684=VERTEX_POINT('',#8878);
#2685=VERTEX_POINT('',#8880);
#2686=VERTEX_POINT('',#8884);
#2687=VERTEX_POINT('',#8886);
#2688=VERTEX_POINT('',#8890);
#2689=VERTEX_POINT('',#8892);
#2690=VERTEX_POINT('',#8896);
#2691=VERTEX_POINT('',#8898);
#2692=VERTEX_POINT('',#8902);
#2693=VERTEX_POINT('',#8904);
#2694=VERTEX_POINT('',#8908);
#2695=VERTEX_POINT('',#8909);
#2696=VERTEX_POINT('',#8911);
#2697=VERTEX_POINT('',#8913);
#2698=VERTEX_POINT('',#8917);
#2699=VERTEX_POINT('',#8919);
#2700=VERTEX_POINT('',#8923);
#2701=VERTEX_POINT('',#8925);
#2702=VERTEX_POINT('',#8929);
#2703=VERTEX_POINT('',#8931);
#2704=VERTEX_POINT('',#8935);
#2705=VERTEX_POINT('',#8937);
#2706=VERTEX_POINT('',#8941);
#2707=VERTEX_POINT('',#8943);
#2708=VERTEX_POINT('',#8947);
#2709=VERTEX_POINT('',#8949);
#2710=VERTEX_POINT('',#8953);
#2711=VERTEX_POINT('',#8955);
#2712=VERTEX_POINT('',#8959);
#2713=VERTEX_POINT('',#8961);
#2714=VERTEX_POINT('',#8965);
#2715=VERTEX_POINT('',#8967);
#2716=VERTEX_POINT('',#8971);
#2717=VERTEX_POINT('',#8973);
#2718=VERTEX_POINT('',#8977);
#2719=VERTEX_POINT('',#8979);
#2720=VERTEX_POINT('',#8986);
#2721=VERTEX_POINT('',#8988);
#2722=VERTEX_POINT('',#8995);
#2723=VERTEX_POINT('',#8997);
#2724=VERTEX_POINT('',#9010);
#2725=VERTEX_POINT('',#9011);
#2726=VERTEX_POINT('',#9013);
#2727=VERTEX_POINT('',#9015);
#2728=VERTEX_POINT('',#9017);
#2729=VERTEX_POINT('',#9019);
#2730=VERTEX_POINT('',#9023);
#2731=VERTEX_POINT('',#9025);
#2732=VERTEX_POINT('',#9028);
#2733=VERTEX_POINT('',#9030);
#2734=VERTEX_POINT('',#9034);
#2735=VERTEX_POINT('',#9038);
#2736=VERTEX_POINT('',#9042);
#2737=VERTEX_POINT('',#9044);
#2738=VERTEX_POINT('',#9048);
#2739=VERTEX_POINT('',#9050);
#2740=VERTEX_POINT('',#9054);
#2741=VERTEX_POINT('',#9058);
#2742=VERTEX_POINT('',#9066);
#2743=VERTEX_POINT('',#9068);
#2744=VERTEX_POINT('',#9072);
#2745=VERTEX_POINT('',#9076);
#2746=VERTEX_POINT('',#9079);
#2747=VERTEX_POINT('',#9085);
#2748=VERTEX_POINT('',#9086);
#2749=VERTEX_POINT('',#9088);
#2750=VERTEX_POINT('',#9090);
#2751=VERTEX_POINT('',#9094);
#2752=VERTEX_POINT('',#9096);
#2753=VERTEX_POINT('',#9100);
#2754=VERTEX_POINT('',#9102);
#2755=VERTEX_POINT('',#9106);
#2756=VERTEX_POINT('',#9108);
#2757=VERTEX_POINT('',#9112);
#2758=VERTEX_POINT('',#9114);
#2759=VERTEX_POINT('',#9123);
#2760=VERTEX_POINT('',#9126);
#2761=VERTEX_POINT('',#9129);
#2762=VERTEX_POINT('',#9133);
#2763=VERTEX_POINT('',#9137);
#2764=VERTEX_POINT('',#9141);
#2765=VERTEX_POINT('',#9144);
#2766=VERTEX_POINT('',#9151);
#2767=VERTEX_POINT('',#9153);
#2768=VERTEX_POINT('',#9157);
#2769=VERTEX_POINT('',#9162);
#2770=VERTEX_POINT('',#9164);
#2771=VERTEX_POINT('',#9166);
#2772=VERTEX_POINT('',#9170);
#2773=VERTEX_POINT('',#9174);
#2774=VERTEX_POINT('',#9178);
#2775=VERTEX_POINT('',#9182);
#2776=VERTEX_POINT('',#9190);
#2777=VERTEX_POINT('',#9192);
#2778=VERTEX_POINT('',#9196);
#2779=VERTEX_POINT('',#9200);
#2780=VERTEX_POINT('',#9204);
#2781=VERTEX_POINT('',#9208);
#2782=VERTEX_POINT('',#9217);
#2783=VERTEX_POINT('',#9218);
#2784=VERTEX_POINT('',#9222);
#2785=VERTEX_POINT('',#9226);
#2786=VERTEX_POINT('',#9229);
#2787=VERTEX_POINT('',#9233);
#2788=VERTEX_POINT('',#9237);
#2789=VERTEX_POINT('',#9245);
#2790=VERTEX_POINT('',#9247);
#2791=VERTEX_POINT('',#9249);
#2792=VERTEX_POINT('',#9253);
#2793=VERTEX_POINT('',#9257);
#2794=VERTEX_POINT('',#9261);
#2795=VERTEX_POINT('',#9265);
#2796=VERTEX_POINT('',#9280);
#2797=VERTEX_POINT('',#9282);
#2798=VERTEX_POINT('',#9295);
#2799=VERTEX_POINT('',#9297);
#2800=VERTEX_POINT('',#9301);
#2801=VERTEX_POINT('',#9303);
#2802=VERTEX_POINT('',#9307);
#2803=VERTEX_POINT('',#9309);
#2804=VERTEX_POINT('',#9313);
#2805=VERTEX_POINT('',#9315);
#2806=VERTEX_POINT('',#9319);
#2807=VERTEX_POINT('',#9321);
#2808=VERTEX_POINT('',#9325);
#2809=VERTEX_POINT('',#9328);
#2810=VERTEX_POINT('',#9332);
#2811=VERTEX_POINT('',#9334);
#2812=VERTEX_POINT('',#9341);
#2813=VERTEX_POINT('',#9343);
#2814=VERTEX_POINT('',#9347);
#2815=VERTEX_POINT('',#9349);
#2816=VERTEX_POINT('',#9353);
#2817=VERTEX_POINT('',#9355);
#2818=VERTEX_POINT('',#9359);
#2819=VERTEX_POINT('',#9361);
#2820=VERTEX_POINT('',#9365);
#2821=VERTEX_POINT('',#9367);
#2822=VERTEX_POINT('',#9371);
#2823=VERTEX_POINT('',#9374);
#2824=VERTEX_POINT('',#9378);
#2825=VERTEX_POINT('',#9380);
#2826=VERTEX_POINT('',#9387);
#2827=VERTEX_POINT('',#9389);
#2828=VERTEX_POINT('',#9393);
#2829=VERTEX_POINT('',#9395);
#2830=VERTEX_POINT('',#9402);
#2831=VERTEX_POINT('',#9404);
#2832=VERTEX_POINT('',#9408);
#2833=VERTEX_POINT('',#9410);
#2834=VERTEX_POINT('',#9414);
#2835=VERTEX_POINT('',#9416);
#2836=VERTEX_POINT('',#9420);
#2837=VERTEX_POINT('',#9422);
#2838=VERTEX_POINT('',#9426);
#2839=VERTEX_POINT('',#9428);
#2840=VERTEX_POINT('',#9432);
#2841=VERTEX_POINT('',#9434);
#2842=VERTEX_POINT('',#9441);
#2843=VERTEX_POINT('',#9444);
#2844=VERTEX_POINT('',#9448);
#2845=VERTEX_POINT('',#9452);
#2846=VERTEX_POINT('',#9456);
#2847=VERTEX_POINT('',#9459);
#2848=VERTEX_POINT('',#9463);
#2849=VERTEX_POINT('',#9467);
#2850=VERTEX_POINT('',#9472);
#2851=VERTEX_POINT('',#9473);
#2852=VERTEX_POINT('',#9475);
#2853=VERTEX_POINT('',#9477);
#2854=VERTEX_POINT('',#9481);
#2855=VERTEX_POINT('',#9483);
#2856=VERTEX_POINT('',#9487);
#2857=VERTEX_POINT('',#9489);
#2858=VERTEX_POINT('',#9493);
#2859=VERTEX_POINT('',#9495);
#2860=VERTEX_POINT('',#9499);
#2861=VERTEX_POINT('',#9501);
#2862=EDGE_CURVE('',#2420,#2420,#2208,.T.);
#2863=EDGE_CURVE('',#2420,#2421,#1398,.T.);
#2864=EDGE_CURVE('',#2421,#2421,#2209,.T.);
#2865=EDGE_CURVE('',#2422,#2422,#2210,.T.);
#2866=EDGE_CURVE('',#2422,#2423,#1399,.T.);
#2867=EDGE_CURVE('',#2423,#2423,#2211,.T.);
#2868=EDGE_CURVE('',#2424,#2424,#2212,.T.);
#2869=EDGE_CURVE('',#2425,#2425,#2213,.T.);
#2870=EDGE_CURVE('',#2426,#2426,#2214,.T.);
#2871=EDGE_CURVE('',#2427,#2427,#2215,.T.);
#2872=EDGE_CURVE('',#2424,#2426,#1400,.T.);
#2873=EDGE_CURVE('',#2427,#2428,#1401,.T.);
#2874=EDGE_CURVE('',#2428,#2428,#2216,.T.);
#2875=EDGE_CURVE('',#2429,#2429,#2217,.T.);
#2876=EDGE_CURVE('',#2429,#2425,#1402,.T.);
#2877=EDGE_CURVE('',#2430,#2430,#2218,.T.);
#2878=EDGE_CURVE('',#2430,#2431,#1403,.T.);
#2879=EDGE_CURVE('',#2431,#2431,#2219,.T.);
#2880=EDGE_CURVE('',#2432,#2432,#2220,.T.);
#2881=EDGE_CURVE('',#2432,#2433,#1404,.T.);
#2882=EDGE_CURVE('',#2433,#2433,#2221,.T.);
#2883=EDGE_CURVE('',#2434,#2434,#2222,.T.);
#2884=EDGE_CURVE('',#2434,#2435,#1405,.T.);
#2885=EDGE_CURVE('',#2435,#2435,#2223,.T.);
#2886=EDGE_CURVE('',#2436,#2436,#2224,.T.);
#2887=EDGE_CURVE('',#2436,#2437,#1406,.T.);
#2888=EDGE_CURVE('',#2437,#2437,#2225,.T.);
#2889=EDGE_CURVE('',#2438,#2438,#2226,.T.);
#2890=EDGE_CURVE('',#2438,#2439,#1407,.T.);
#2891=EDGE_CURVE('',#2439,#2439,#2227,.T.);
#2892=EDGE_CURVE('',#2440,#2440,#2228,.T.);
#2893=EDGE_CURVE('',#2440,#2441,#1408,.T.);
#2894=EDGE_CURVE('',#2441,#2441,#2229,.T.);
#2895=EDGE_CURVE('',#2442,#2442,#2230,.T.);
#2896=EDGE_CURVE('',#2442,#2443,#1409,.T.);
#2897=EDGE_CURVE('',#2443,#2443,#2231,.T.);
#2898=EDGE_CURVE('',#2444,#2444,#2232,.T.);
#2899=EDGE_CURVE('',#2444,#2445,#1410,.T.);
#2900=EDGE_CURVE('',#2445,#2445,#2233,.T.);
#2901=EDGE_CURVE('',#2446,#2447,#2234,.T.);
#2902=EDGE_CURVE('',#2447,#2446,#2235,.T.);
#2903=EDGE_CURVE('',#2447,#2448,#2236,.T.);
#2904=EDGE_CURVE('',#2449,#2448,#2237,.T.);
#2905=EDGE_CURVE('',#2448,#2449,#2238,.T.);
#2906=EDGE_CURVE('',#2449,#2450,#1411,.T.);
#2907=EDGE_CURVE('',#2450,#2450,#2239,.T.);
#2908=EDGE_CURVE('',#2451,#2451,#2240,.T.);
#2909=EDGE_CURVE('',#2451,#2452,#1412,.T.);
#2910=EDGE_CURVE('',#2452,#2452,#2241,.T.);
#2911=EDGE_CURVE('',#2452,#2453,#1413,.T.);
#2912=EDGE_CURVE('',#2453,#2453,#2242,.T.);
#2913=EDGE_CURVE('',#2454,#2454,#2243,.T.);
#2914=EDGE_CURVE('',#2454,#2446,#1414,.T.);
#2915=EDGE_CURVE('',#2455,#2455,#2244,.T.);
#2916=EDGE_CURVE('',#2455,#2451,#1415,.T.);
#2917=EDGE_CURVE('',#2456,#2457,#2245,.T.);
#2918=EDGE_CURVE('',#2457,#2456,#2246,.T.);
#2919=EDGE_CURVE('',#2457,#2458,#2247,.T.);
#2920=EDGE_CURVE('',#2459,#2458,#2248,.T.);
#2921=EDGE_CURVE('',#2458,#2459,#2249,.T.);
#2922=EDGE_CURVE('',#2460,#2460,#2250,.T.);
#2923=EDGE_CURVE('',#2460,#2459,#1416,.T.);
#2924=EDGE_CURVE('',#2461,#2461,#2251,.T.);
#2925=EDGE_CURVE('',#2462,#2462,#2252,.T.);
#2926=EDGE_CURVE('',#2463,#2463,#2253,.T.);
#2927=EDGE_CURVE('',#2463,#2461,#1417,.T.);
#2928=EDGE_CURVE('',#2464,#2464,#2254,.T.);
#2929=EDGE_CURVE('',#2464,#2463,#1418,.T.);
#2930=EDGE_CURVE('',#2465,#2465,#2255,.T.);
#2931=EDGE_CURVE('',#2465,#2464,#1419,.T.);
#2932=EDGE_CURVE('',#2456,#2462,#1420,.T.);
#2933=EDGE_CURVE('',#2466,#2467,#2256,.T.);
#2934=EDGE_CURVE('',#2468,#2469,#2257,.T.);
#2935=EDGE_CURVE('',#2470,#2471,#2258,.T.);
#2936=EDGE_CURVE('',#2472,#2473,#2259,.T.);
#2937=EDGE_CURVE('',#2474,#2475,#2260,.T.);
#2938=EDGE_CURVE('',#2476,#2477,#2261,.T.);
#2939=EDGE_CURVE('',#2478,#2479,#2262,.T.);
#2940=EDGE_CURVE('',#2480,#2481,#2263,.T.);
#2941=EDGE_CURVE('',#2482,#2483,#271,.T.);
#2942=EDGE_CURVE('',#2484,#2482,#2264,.T.);
#2943=EDGE_CURVE('',#2485,#2484,#272,.T.);
#2944=EDGE_CURVE('',#2483,#2485,#2265,.T.);
#2945=EDGE_CURVE('',#2486,#2484,#2266,.T.);
#2946=EDGE_CURVE('',#2486,#2487,#273,.T.);
#2947=EDGE_CURVE('',#2488,#2487,#2267,.T.);
#2948=EDGE_CURVE('',#2488,#2489,#274,.T.);
#2949=EDGE_CURVE('',#2490,#2489,#2268,.T.);
#2950=EDGE_CURVE('',#2490,#2491,#275,.T.);
#2951=EDGE_CURVE('',#2491,#2492,#1421,.T.);
#2952=EDGE_CURVE('',#2492,#2492,#2269,.T.);
#2953=EDGE_CURVE('',#2491,#2493,#276,.T.);
#2954=EDGE_CURVE('',#2494,#2493,#2270,.T.);
#2955=EDGE_CURVE('',#2494,#2495,#277,.T.);
#2956=EDGE_CURVE('',#2496,#2495,#2271,.T.);
#2957=EDGE_CURVE('',#2496,#2497,#278,.T.);
#2958=EDGE_CURVE('',#2498,#2497,#2272,.T.);
#2959=EDGE_CURVE('',#2498,#2499,#279,.T.);
#2960=EDGE_CURVE('',#2500,#2499,#2273,.T.);
#2961=EDGE_CURVE('',#2500,#2501,#280,.T.);
#2962=EDGE_CURVE('',#2485,#2501,#2274,.T.);
#2963=EDGE_CURVE('',#2482,#2502,#2275,.T.);
#2964=EDGE_CURVE('',#2502,#2486,#2276,.T.);
#2965=EDGE_CURVE('',#2503,#2502,#281,.T.);
#2966=EDGE_CURVE('',#2487,#2503,#2277,.T.);
#2967=EDGE_CURVE('',#2503,#2504,#2278,.T.);
#2968=EDGE_CURVE('',#2504,#2488,#2279,.T.);
#2969=EDGE_CURVE('',#2505,#2504,#282,.T.);
#2970=EDGE_CURVE('',#2489,#2505,#2280,.T.);
#2971=EDGE_CURVE('',#2505,#2506,#2281,.T.);
#2972=EDGE_CURVE('',#2506,#2490,#2282,.T.);
#2973=EDGE_CURVE('',#2507,#2508,#283,.T.);
#2974=EDGE_CURVE('',#2493,#2507,#2283,.T.);
#2975=EDGE_CURVE('',#2508,#2506,#284,.T.);
#2976=EDGE_CURVE('',#2507,#2509,#2284,.T.);
#2977=EDGE_CURVE('',#2509,#2494,#2285,.T.);
#2978=EDGE_CURVE('',#2510,#2509,#285,.T.);
#2979=EDGE_CURVE('',#2495,#2510,#2286,.T.);
#2980=EDGE_CURVE('',#2510,#2511,#2287,.T.);
#2981=EDGE_CURVE('',#2511,#2496,#2288,.T.);
#2982=EDGE_CURVE('',#2512,#2511,#286,.T.);
#2983=EDGE_CURVE('',#2497,#2512,#2289,.T.);
#2984=EDGE_CURVE('',#2512,#2513,#2290,.T.);
#2985=EDGE_CURVE('',#2513,#2498,#2291,.T.);
#2986=EDGE_CURVE('',#2514,#2513,#287,.T.);
#2987=EDGE_CURVE('',#2499,#2514,#2292,.T.);
#2988=EDGE_CURVE('',#2515,#2515,#2293,.T.);
#2989=EDGE_CURVE('',#2515,#2508,#1422,.T.);
#2990=EDGE_CURVE('',#2516,#2483,#2294,.T.);
#2991=EDGE_CURVE('',#2516,#2517,#288,.T.);
#2992=EDGE_CURVE('',#2514,#2517,#2295,.T.);
#2993=EDGE_CURVE('',#2501,#2516,#2296,.T.);
#2994=EDGE_CURVE('',#2517,#2500,#2297,.T.);
#2995=EDGE_CURVE('',#2518,#2518,#2298,.T.);
#2996=EDGE_CURVE('',#2519,#2519,#2299,.T.);
#2997=EDGE_CURVE('',#2520,#2520,#2300,.T.);
#2998=EDGE_CURVE('',#2520,#2518,#1423,.T.);
#2999=EDGE_CURVE('',#2521,#2521,#2301,.T.);
#3000=EDGE_CURVE('',#2521,#2519,#1424,.T.);
#3001=EDGE_CURVE('',#2522,#2522,#2302,.T.);
#3002=EDGE_CURVE('',#2523,#2523,#2303,.T.);
#3003=EDGE_CURVE('',#2524,#2524,#2304,.T.);
#3004=EDGE_CURVE('',#2524,#2522,#1425,.T.);
#3005=EDGE_CURVE('',#2525,#2525,#2305,.T.);
#3006=EDGE_CURVE('',#2525,#2523,#1426,.T.);
#3007=EDGE_CURVE('',#2526,#2527,#1427,.T.);
#3008=EDGE_CURVE('',#2528,#2526,#2306,.T.);
#3009=EDGE_CURVE('',#2529,#2528,#1428,.T.);
#3010=EDGE_CURVE('',#2527,#2529,#2307,.T.);
#3011=EDGE_CURVE('',#2530,#2531,#1429,.T.);
#3012=EDGE_CURVE('',#2532,#2530,#2308,.T.);
#3013=EDGE_CURVE('',#2533,#2532,#1430,.T.);
#3014=EDGE_CURVE('',#2531,#2533,#2309,.T.);
#3015=EDGE_CURVE('',#2534,#2527,#1431,.T.);
#3016=EDGE_CURVE('',#2534,#2535,#1432,.T.);
#3017=EDGE_CURVE('',#2535,#2526,#1433,.T.);
#3018=EDGE_CURVE('',#2531,#2536,#1434,.T.);
#3019=EDGE_CURVE('',#2536,#2537,#1435,.T.);
#3020=EDGE_CURVE('',#2530,#2537,#1436,.T.);
#3021=EDGE_CURVE('',#2538,#2538,#2310,.T.);
#3022=EDGE_CURVE('',#2535,#2539,#1437,.T.);
#3023=EDGE_CURVE('',#2528,#2539,#1438,.T.);
#3024=EDGE_CURVE('',#2540,#2533,#1439,.T.);
#3025=EDGE_CURVE('',#2540,#2536,#2311,.T.);
#3026=EDGE_CURVE('',#2539,#2541,#1440,.T.);
#3027=EDGE_CURVE('',#2529,#2541,#1441,.T.);
#3028=EDGE_CURVE('',#2542,#2532,#1442,.T.);
#3029=EDGE_CURVE('',#2542,#2540,#1443,.T.);
#3030=EDGE_CURVE('',#2543,#2543,#2312,.T.);
#3031=EDGE_CURVE('',#2544,#2544,#2313,.T.);
#3032=EDGE_CURVE('',#2544,#2545,#1444,.T.);
#3033=EDGE_CURVE('',#2545,#2545,#2314,.T.);
#3034=EDGE_CURVE('',#2546,#2547,#1445,.T.);
#3035=EDGE_CURVE('',#2548,#2546,#2315,.T.);
#3036=EDGE_CURVE('',#2549,#2548,#1446,.T.);
#3037=EDGE_CURVE('',#2547,#2549,#2316,.T.);
#3038=EDGE_CURVE('',#2537,#2542,#2317,.T.);
#3039=EDGE_CURVE('',#2550,#2547,#1447,.T.);
#3040=EDGE_CURVE('',#2550,#2551,#1448,.T.);
#3041=EDGE_CURVE('',#2551,#2546,#1449,.T.);
#3042=EDGE_CURVE('',#2552,#2551,#1450,.T.);
#3043=EDGE_CURVE('',#2548,#2552,#1451,.T.);
#3044=EDGE_CURVE('',#2552,#2553,#1452,.T.);
#3045=EDGE_CURVE('',#2549,#2553,#1453,.T.);
#3046=EDGE_CURVE('',#2554,#2554,#2318,.T.);
#3047=EDGE_CURVE('',#2554,#2555,#1454,.T.);
#3048=EDGE_CURVE('',#2555,#2555,#2319,.T.);
#3049=EDGE_CURVE('',#2538,#2543,#1455,.T.);
#3050=EDGE_CURVE('',#2541,#2534,#1456,.T.);
#3051=EDGE_CURVE('',#2553,#2550,#1457,.T.);
#3052=EDGE_CURVE('',#2556,#2557,#1458,.T.);
#3053=EDGE_CURVE('',#2557,#2558,#1459,.T.);
#3054=EDGE_CURVE('',#2559,#2558,#1460,.T.);
#3055=EDGE_CURVE('',#2556,#2559,#1461,.T.);
#3056=EDGE_CURVE('',#2560,#2556,#1462,.T.);
#3057=EDGE_CURVE('',#2561,#2559,#1463,.T.);
#3058=EDGE_CURVE('',#2560,#2561,#1464,.T.);
#3059=EDGE_CURVE('',#2562,#2560,#1465,.T.);
#3060=EDGE_CURVE('',#2563,#2561,#1466,.T.);
#3061=EDGE_CURVE('',#2562,#2563,#1467,.T.);
#3062=EDGE_CURVE('',#2557,#2562,#1468,.T.);
#3063=EDGE_CURVE('',#2558,#2563,#1469,.T.);
#3064=EDGE_CURVE('',#2564,#2564,#2320,.T.);
#3065=EDGE_CURVE('',#2564,#2565,#1470,.T.);
#3066=EDGE_CURVE('',#2565,#2565,#2321,.T.);
#3067=EDGE_CURVE('',#2566,#2566,#2322,.T.);
#3068=EDGE_CURVE('',#2566,#2567,#1471,.T.);
#3069=EDGE_CURVE('',#2567,#2567,#2323,.T.);
#3070=EDGE_CURVE('',#2568,#2569,#1472,.T.);
#3071=EDGE_CURVE('',#2569,#2570,#1473,.T.);
#3072=EDGE_CURVE('',#2571,#2570,#1474,.T.);
#3073=EDGE_CURVE('',#2568,#2571,#1475,.T.);
#3074=EDGE_CURVE('',#2572,#2573,#1476,.T.);
#3075=EDGE_CURVE('',#2572,#2571,#1477,.T.);
#3076=EDGE_CURVE('',#2570,#2573,#1478,.T.);
#3077=EDGE_CURVE('',#2573,#2574,#1479,.T.);
#3078=EDGE_CURVE('',#2574,#2575,#1480,.T.);
#3079=EDGE_CURVE('',#2575,#2572,#1481,.T.);
#3080=EDGE_CURVE('',#2576,#2569,#1482,.T.);
#3081=EDGE_CURVE('',#2576,#2577,#1483,.T.);
#3082=EDGE_CURVE('',#2577,#2574,#1484,.T.);
#3083=EDGE_CURVE('',#2578,#2575,#1485,.T.);
#3084=EDGE_CURVE('',#2578,#2579,#1486,.T.);
#3085=EDGE_CURVE('',#2579,#2568,#1487,.T.);
#3086=EDGE_CURVE('',#2577,#2578,#1488,.T.);
#3087=EDGE_CURVE('',#2579,#2576,#1489,.T.);
#3088=EDGE_CURVE('',#2580,#2581,#1490,.T.);
#3089=EDGE_CURVE('',#2582,#2580,#2324,.T.);
#3090=EDGE_CURVE('',#2583,#2582,#1491,.T.);
#3091=EDGE_CURVE('',#2581,#2583,#2325,.T.);
#3092=EDGE_CURVE('',#2584,#2585,#1492,.T.);
#3093=EDGE_CURVE('',#2586,#2584,#2326,.T.);
#3094=EDGE_CURVE('',#2587,#2586,#1493,.T.);
#3095=EDGE_CURVE('',#2585,#2587,#2327,.T.);
#3096=EDGE_CURVE('',#2588,#2581,#1494,.T.);
#3097=EDGE_CURVE('',#2588,#2589,#1495,.T.);
#3098=EDGE_CURVE('',#2589,#2580,#1496,.T.);
#3099=EDGE_CURVE('',#2585,#2590,#1497,.T.);
#3100=EDGE_CURVE('',#2590,#2591,#1498,.T.);
#3101=EDGE_CURVE('',#2584,#2591,#1499,.T.);
#3102=EDGE_CURVE('',#2592,#2592,#2328,.T.);
#3103=EDGE_CURVE('',#2589,#2593,#1500,.T.);
#3104=EDGE_CURVE('',#2582,#2593,#1501,.T.);
#3105=EDGE_CURVE('',#2594,#2587,#1502,.T.);
#3106=EDGE_CURVE('',#2594,#2590,#2329,.T.);
#3107=EDGE_CURVE('',#2593,#2595,#1503,.T.);
#3108=EDGE_CURVE('',#2583,#2595,#1504,.T.);
#3109=EDGE_CURVE('',#2596,#2586,#1505,.T.);
#3110=EDGE_CURVE('',#2596,#2594,#1506,.T.);
#3111=EDGE_CURVE('',#2597,#2597,#2330,.T.);
#3112=EDGE_CURVE('',#2598,#2598,#2331,.T.);
#3113=EDGE_CURVE('',#2598,#2599,#1507,.T.);
#3114=EDGE_CURVE('',#2599,#2599,#2332,.T.);
#3115=EDGE_CURVE('',#2600,#2601,#1508,.T.);
#3116=EDGE_CURVE('',#2602,#2600,#2333,.T.);
#3117=EDGE_CURVE('',#2603,#2602,#1509,.T.);
#3118=EDGE_CURVE('',#2601,#2603,#2334,.T.);
#3119=EDGE_CURVE('',#2591,#2596,#2335,.T.);
#3120=EDGE_CURVE('',#2604,#2601,#1510,.T.);
#3121=EDGE_CURVE('',#2604,#2605,#1511,.T.);
#3122=EDGE_CURVE('',#2605,#2600,#1512,.T.);
#3123=EDGE_CURVE('',#2606,#2605,#1513,.T.);
#3124=EDGE_CURVE('',#2602,#2606,#1514,.T.);
#3125=EDGE_CURVE('',#2606,#2607,#1515,.T.);
#3126=EDGE_CURVE('',#2603,#2607,#1516,.T.);
#3127=EDGE_CURVE('',#2608,#2608,#2336,.T.);
#3128=EDGE_CURVE('',#2608,#2609,#1517,.T.);
#3129=EDGE_CURVE('',#2609,#2609,#2337,.T.);
#3130=EDGE_CURVE('',#2592,#2597,#1518,.T.);
#3131=EDGE_CURVE('',#2595,#2588,#1519,.T.);
#3132=EDGE_CURVE('',#2607,#2604,#1520,.T.);
#3133=EDGE_CURVE('',#2610,#2611,#1521,.T.);
#3134=EDGE_CURVE('',#2611,#2612,#1522,.T.);
#3135=EDGE_CURVE('',#2613,#2612,#1523,.T.);
#3136=EDGE_CURVE('',#2610,#2613,#1524,.T.);
#3137=EDGE_CURVE('',#2614,#2610,#1525,.T.);
#3138=EDGE_CURVE('',#2615,#2613,#1526,.T.);
#3139=EDGE_CURVE('',#2614,#2615,#1527,.T.);
#3140=EDGE_CURVE('',#2616,#2614,#1528,.T.);
#3141=EDGE_CURVE('',#2617,#2615,#1529,.T.);
#3142=EDGE_CURVE('',#2616,#2617,#1530,.T.);
#3143=EDGE_CURVE('',#2611,#2616,#1531,.T.);
#3144=EDGE_CURVE('',#2612,#2617,#1532,.T.);
#3145=EDGE_CURVE('',#2618,#2618,#2338,.T.);
#3146=EDGE_CURVE('',#2618,#2619,#1533,.T.);
#3147=EDGE_CURVE('',#2619,#2619,#2339,.T.);
#3148=EDGE_CURVE('',#2620,#2620,#2340,.T.);
#3149=EDGE_CURVE('',#2620,#2621,#1534,.T.);
#3150=EDGE_CURVE('',#2621,#2621,#2341,.T.);
#3151=EDGE_CURVE('',#2622,#2623,#1535,.T.);
#3152=EDGE_CURVE('',#2623,#2624,#1536,.T.);
#3153=EDGE_CURVE('',#2625,#2624,#1537,.T.);
#3154=EDGE_CURVE('',#2622,#2625,#1538,.T.);
#3155=EDGE_CURVE('',#2626,#2627,#1539,.T.);
#3156=EDGE_CURVE('',#2626,#2625,#1540,.T.);
#3157=EDGE_CURVE('',#2624,#2627,#1541,.T.);
#3158=EDGE_CURVE('',#2627,#2628,#1542,.T.);
#3159=EDGE_CURVE('',#2628,#2629,#1543,.T.);
#3160=EDGE_CURVE('',#2629,#2626,#1544,.T.);
#3161=EDGE_CURVE('',#2630,#2623,#1545,.T.);
#3162=EDGE_CURVE('',#2630,#2631,#1546,.T.);
#3163=EDGE_CURVE('',#2631,#2628,#1547,.T.);
#3164=EDGE_CURVE('',#2632,#2629,#1548,.T.);
#3165=EDGE_CURVE('',#2632,#2633,#1549,.T.);
#3166=EDGE_CURVE('',#2633,#2622,#1550,.T.);
#3167=EDGE_CURVE('',#2631,#2632,#1551,.T.);
#3168=EDGE_CURVE('',#2633,#2630,#1552,.T.);
#3169=EDGE_CURVE('',#2634,#2635,#1553,.T.);
#3170=EDGE_CURVE('',#2634,#2636,#1554,.T.);
#3171=EDGE_CURVE('',#2637,#2636,#1555,.T.);
#3172=EDGE_CURVE('',#2635,#2637,#1556,.T.);
#3173=EDGE_CURVE('',#2638,#2634,#1557,.T.);
#3174=EDGE_CURVE('',#2638,#2639,#1558,.T.);
#3175=EDGE_CURVE('',#2636,#2639,#1559,.T.);
#3176=EDGE_CURVE('',#2640,#2638,#1560,.T.);
#3177=EDGE_CURVE('',#2640,#2641,#1561,.T.);
#3178=EDGE_CURVE('',#2639,#2641,#1562,.T.);
#3179=EDGE_CURVE('',#2642,#2640,#1563,.T.);
#3180=EDGE_CURVE('',#2642,#2643,#1564,.T.);
#3181=EDGE_CURVE('',#2641,#2643,#1565,.T.);
#3182=EDGE_CURVE('',#2644,#2642,#1566,.T.);
#3183=EDGE_CURVE('',#2644,#2645,#1567,.T.);
#3184=EDGE_CURVE('',#2643,#2645,#1568,.T.);
#3185=EDGE_CURVE('',#2646,#2644,#1569,.T.);
#3186=EDGE_CURVE('',#2646,#2647,#1570,.T.);
#3187=EDGE_CURVE('',#2645,#2647,#1571,.T.);
#3188=EDGE_CURVE('',#2648,#2646,#1572,.T.);
#3189=EDGE_CURVE('',#2648,#2649,#1573,.T.);
#3190=EDGE_CURVE('',#2647,#2649,#1574,.T.);
#3191=EDGE_CURVE('',#2650,#2648,#1575,.T.);
#3192=EDGE_CURVE('',#2650,#2651,#1576,.T.);
#3193=EDGE_CURVE('',#2649,#2651,#1577,.T.);
#3194=EDGE_CURVE('',#2652,#2650,#1578,.T.);
#3195=EDGE_CURVE('',#2653,#2652,#1579,.T.);
#3196=EDGE_CURVE('',#2651,#2653,#1580,.T.);
#3197=EDGE_CURVE('',#2654,#2655,#1581,.T.);
#3198=EDGE_CURVE('',#2654,#2656,#1582,.T.);
#3199=EDGE_CURVE('',#2657,#2656,#1583,.T.);
#3200=EDGE_CURVE('',#2655,#2657,#1584,.T.);
#3201=EDGE_CURVE('',#2658,#2654,#1585,.T.);
#3202=EDGE_CURVE('',#2658,#2659,#1586,.T.);
#3203=EDGE_CURVE('',#2656,#2659,#1587,.T.);
#3204=EDGE_CURVE('',#2660,#2658,#1588,.T.);
#3205=EDGE_CURVE('',#2660,#2661,#1589,.T.);
#3206=EDGE_CURVE('',#2659,#2661,#1590,.T.);
#3207=EDGE_CURVE('',#2662,#2660,#1591,.T.);
#3208=EDGE_CURVE('',#2662,#2663,#1592,.T.);
#3209=EDGE_CURVE('',#2661,#2663,#1593,.T.);
#3210=EDGE_CURVE('',#2664,#2662,#1594,.T.);
#3211=EDGE_CURVE('',#2664,#2665,#1595,.T.);
#3212=EDGE_CURVE('',#2663,#2665,#1596,.T.);
#3213=EDGE_CURVE('',#2666,#2664,#1597,.T.);
#3214=EDGE_CURVE('',#2666,#2667,#1598,.T.);
#3215=EDGE_CURVE('',#2665,#2667,#1599,.T.);
#3216=EDGE_CURVE('',#2668,#2666,#1600,.T.);
#3217=EDGE_CURVE('',#2668,#2669,#1601,.T.);
#3218=EDGE_CURVE('',#2667,#2669,#1602,.T.);
#3219=EDGE_CURVE('',#2670,#2668,#1603,.T.);
#3220=EDGE_CURVE('',#2670,#2671,#1604,.T.);
#3221=EDGE_CURVE('',#2669,#2671,#1605,.T.);
#3222=EDGE_CURVE('',#2672,#2670,#1606,.T.);
#3223=EDGE_CURVE('',#2673,#2672,#1607,.T.);
#3224=EDGE_CURVE('',#2671,#2673,#1608,.T.);
#3225=EDGE_CURVE('',#2674,#2675,#1609,.T.);
#3226=EDGE_CURVE('',#2674,#2676,#1610,.T.);
#3227=EDGE_CURVE('',#2677,#2676,#1611,.T.);
#3228=EDGE_CURVE('',#2675,#2677,#1612,.T.);
#3229=EDGE_CURVE('',#2678,#2674,#1613,.T.);
#3230=EDGE_CURVE('',#2678,#2679,#1614,.T.);
#3231=EDGE_CURVE('',#2676,#2679,#1615,.T.);
#3232=EDGE_CURVE('',#2680,#2678,#1616,.T.);
#3233=EDGE_CURVE('',#2680,#2681,#1617,.T.);
#3234=EDGE_CURVE('',#2679,#2681,#1618,.T.);
#3235=EDGE_CURVE('',#2682,#2680,#1619,.T.);
#3236=EDGE_CURVE('',#2682,#2683,#1620,.T.);
#3237=EDGE_CURVE('',#2681,#2683,#1621,.T.);
#3238=EDGE_CURVE('',#2684,#2682,#1622,.T.);
#3239=EDGE_CURVE('',#2684,#2685,#1623,.T.);
#3240=EDGE_CURVE('',#2683,#2685,#1624,.T.);
#3241=EDGE_CURVE('',#2686,#2684,#1625,.T.);
#3242=EDGE_CURVE('',#2686,#2687,#1626,.T.);
#3243=EDGE_CURVE('',#2685,#2687,#1627,.T.);
#3244=EDGE_CURVE('',#2688,#2686,#1628,.T.);
#3245=EDGE_CURVE('',#2688,#2689,#1629,.T.);
#3246=EDGE_CURVE('',#2687,#2689,#1630,.T.);
#3247=EDGE_CURVE('',#2690,#2688,#1631,.T.);
#3248=EDGE_CURVE('',#2690,#2691,#1632,.T.);
#3249=EDGE_CURVE('',#2689,#2691,#1633,.T.);
#3250=EDGE_CURVE('',#2692,#2690,#1634,.T.);
#3251=EDGE_CURVE('',#2693,#2692,#1635,.T.);
#3252=EDGE_CURVE('',#2691,#2693,#1636,.T.);
#3253=EDGE_CURVE('',#2694,#2695,#1637,.T.);
#3254=EDGE_CURVE('',#2694,#2696,#1638,.T.);
#3255=EDGE_CURVE('',#2697,#2696,#1639,.T.);
#3256=EDGE_CURVE('',#2695,#2697,#1640,.T.);
#3257=EDGE_CURVE('',#2698,#2694,#1641,.T.);
#3258=EDGE_CURVE('',#2698,#2699,#1642,.T.);
#3259=EDGE_CURVE('',#2696,#2699,#1643,.T.);
#3260=EDGE_CURVE('',#2700,#2698,#1644,.T.);
#3261=EDGE_CURVE('',#2700,#2701,#1645,.T.);
#3262=EDGE_CURVE('',#2699,#2701,#1646,.T.);
#3263=EDGE_CURVE('',#2702,#2700,#1647,.T.);
#3264=EDGE_CURVE('',#2702,#2703,#1648,.T.);
#3265=EDGE_CURVE('',#2701,#2703,#1649,.T.);
#3266=EDGE_CURVE('',#2704,#2702,#1650,.T.);
#3267=EDGE_CURVE('',#2704,#2705,#1651,.T.);
#3268=EDGE_CURVE('',#2703,#2705,#1652,.T.);
#3269=EDGE_CURVE('',#2706,#2704,#1653,.T.);
#3270=EDGE_CURVE('',#2706,#2707,#1654,.T.);
#3271=EDGE_CURVE('',#2705,#2707,#1655,.T.);
#3272=EDGE_CURVE('',#2708,#2706,#1656,.T.);
#3273=EDGE_CURVE('',#2708,#2709,#1657,.T.);
#3274=EDGE_CURVE('',#2707,#2709,#1658,.T.);
#3275=EDGE_CURVE('',#2710,#2708,#1659,.T.);
#3276=EDGE_CURVE('',#2710,#2711,#1660,.T.);
#3277=EDGE_CURVE('',#2709,#2711,#1661,.T.);
#3278=EDGE_CURVE('',#2712,#2710,#1662,.T.);
#3279=EDGE_CURVE('',#2713,#2712,#1663,.T.);
#3280=EDGE_CURVE('',#2711,#2713,#1664,.T.);
#3281=EDGE_CURVE('',#2714,#2714,#2342,.T.);
#3282=EDGE_CURVE('',#2714,#2715,#1665,.T.);
#3283=EDGE_CURVE('',#2715,#2715,#2343,.T.);
#3284=EDGE_CURVE('',#2652,#2716,#1666,.T.);
#3285=EDGE_CURVE('',#2716,#2717,#1667,.T.);
#3286=EDGE_CURVE('',#2653,#2717,#1668,.T.);
#3287=EDGE_CURVE('',#2718,#2637,#1669,.T.);
#3288=EDGE_CURVE('',#2719,#2718,#1670,.T.);
#3289=EDGE_CURVE('',#2719,#2635,#1671,.T.);
#3290=EDGE_CURVE('',#2672,#2719,#1672,.T.);
#3291=EDGE_CURVE('',#2673,#2718,#1673,.T.);
#3292=EDGE_CURVE('',#2720,#2657,#1674,.T.);
#3293=EDGE_CURVE('',#2721,#2720,#1675,.T.);
#3294=EDGE_CURVE('',#2721,#2655,#1676,.T.);
#3295=EDGE_CURVE('',#2692,#2721,#1677,.T.);
#3296=EDGE_CURVE('',#2693,#2720,#1678,.T.);
#3297=EDGE_CURVE('',#2722,#2677,#1679,.T.);
#3298=EDGE_CURVE('',#2723,#2722,#1680,.T.);
#3299=EDGE_CURVE('',#2723,#2675,#1681,.T.);
#3300=EDGE_CURVE('',#2712,#2723,#1682,.T.);
#3301=EDGE_CURVE('',#2713,#2722,#1683,.T.);
#3302=EDGE_CURVE('',#2717,#2697,#1684,.T.);
#3303=EDGE_CURVE('',#2716,#2695,#1685,.T.);
#3304=EDGE_CURVE('',#2724,#2725,#1686,.T.);
#3305=EDGE_CURVE('',#2725,#2726,#1687,.T.);
#3306=EDGE_CURVE('',#2726,#2727,#1688,.T.);
#3307=EDGE_CURVE('',#2727,#2728,#1689,.T.);
#3308=EDGE_CURVE('',#2728,#2729,#33,.T.);
#3309=EDGE_CURVE('',#2729,#2724,#1690,.T.);
#3310=EDGE_CURVE('',#2730,#2728,#2344,.F.);
#3311=EDGE_CURVE('',#2730,#2731,#1691,.T.);
#3312=EDGE_CURVE('',#2731,#2731,#2345,.T.);
#3313=EDGE_CURVE('',#2732,#2730,#2346,.F.);
#3314=EDGE_CURVE('',#2733,#2732,#34,.T.);
#3315=EDGE_CURVE('',#2729,#2733,#2347,.F.);
#3316=EDGE_CURVE('',#2734,#2727,#1692,.T.);
#3317=EDGE_CURVE('',#2732,#2734,#1693,.T.);
#3318=EDGE_CURVE('',#2735,#2733,#1694,.T.);
#3319=EDGE_CURVE('',#2724,#2735,#1695,.T.);
#3320=EDGE_CURVE('',#2734,#2736,#1696,.T.);
#3321=EDGE_CURVE('',#2736,#2737,#1697,.T.);
#3322=EDGE_CURVE('',#2737,#2735,#1698,.T.);
#3323=EDGE_CURVE('',#2737,#2738,#1699,.T.);
#3324=EDGE_CURVE('',#2739,#2738,#1700,.T.);
#3325=EDGE_CURVE('',#2725,#2739,#1701,.T.);
#3326=EDGE_CURVE('',#2736,#2740,#1702,.T.);
#3327=EDGE_CURVE('',#2738,#2740,#1703,.T.);
#3328=EDGE_CURVE('',#2741,#2739,#1704,.T.);
#3329=EDGE_CURVE('',#2726,#2741,#1705,.T.);
#3330=EDGE_CURVE('',#2740,#2741,#1706,.T.);
#3331=EDGE_CURVE('',#2742,#2742,#2348,.T.);
#3332=EDGE_CURVE('',#2742,#2743,#1707,.T.);
#3333=EDGE_CURVE('',#2743,#2743,#2349,.T.);
#3334=EDGE_CURVE('',#2743,#2744,#1708,.T.);
#3335=EDGE_CURVE('',#2744,#2744,#2350,.T.);
#3336=EDGE_CURVE('',#2745,#2745,#2351,.T.);
#3337=EDGE_CURVE('',#2745,#2746,#1709,.T.);
#3338=EDGE_CURVE('',#2746,#2746,#2352,.T.);
#3339=EDGE_CURVE('',#2747,#2748,#1710,.T.);
#3340=EDGE_CURVE('',#2748,#2749,#1711,.T.);
#3341=EDGE_CURVE('',#2749,#2750,#1712,.T.);
#3342=EDGE_CURVE('',#2747,#2750,#1713,.T.);
#3343=EDGE_CURVE('',#2748,#2751,#1714,.T.);
#3344=EDGE_CURVE('',#2751,#2752,#1715,.T.);
#3345=EDGE_CURVE('',#2752,#2749,#1716,.T.);
#3346=EDGE_CURVE('',#2751,#2753,#1717,.T.);
#3347=EDGE_CURVE('',#2753,#2754,#1718,.T.);
#3348=EDGE_CURVE('',#2754,#2752,#1719,.T.);
#3349=EDGE_CURVE('',#2753,#2755,#1720,.T.);
#3350=EDGE_CURVE('',#2755,#2756,#1721,.T.);
#3351=EDGE_CURVE('',#2756,#2754,#1722,.T.);
#3352=EDGE_CURVE('',#2755,#2757,#1723,.T.);
#3353=EDGE_CURVE('',#2757,#2758,#1724,.T.);
#3354=EDGE_CURVE('',#2758,#2756,#1725,.T.);
#3355=EDGE_CURVE('',#2757,#2747,#1726,.T.);
#3356=EDGE_CURVE('',#2750,#2758,#1727,.T.);
#3357=EDGE_CURVE('',#2759,#2759,#2353,.T.);
#3358=EDGE_CURVE('',#2760,#2760,#2354,.T.);
#3359=EDGE_CURVE('',#2761,#2761,#2355,.T.);
#3360=EDGE_CURVE('',#2761,#2760,#1728,.T.);
#3361=EDGE_CURVE('',#2762,#2762,#2356,.T.);
#3362=EDGE_CURVE('',#2762,#2761,#1729,.T.);
#3363=EDGE_CURVE('',#2763,#2763,#2357,.T.);
#3364=EDGE_CURVE('',#2763,#2762,#1730,.T.);
#3365=EDGE_CURVE('',#2764,#2764,#2358,.T.);
#3366=EDGE_CURVE('',#2765,#2765,#2359,.F.);
#3367=EDGE_CURVE('',#2765,#2764,#1731,.T.);
#3368=EDGE_CURVE('',#2759,#2765,#1732,.T.);
#3369=EDGE_CURVE('',#2766,#2766,#2360,.F.);
#3370=EDGE_CURVE('',#2766,#2767,#1733,.T.);
#3371=EDGE_CURVE('',#2767,#2767,#2361,.F.);
#3372=EDGE_CURVE('',#2768,#2768,#2362,.T.);
#3373=EDGE_CURVE('',#2768,#2766,#1734,.T.);
#3374=EDGE_CURVE('',#2769,#2769,#2363,.T.);
#3375=EDGE_CURVE('',#2769,#2770,#1735,.T.);
#3376=EDGE_CURVE('',#2771,#2770,#11,.T.);
#3377=EDGE_CURVE('',#2772,#2771,#12,.T.);
#3378=EDGE_CURVE('',#2773,#2772,#13,.T.);
#3379=EDGE_CURVE('',#2774,#2773,#14,.T.);
#3380=EDGE_CURVE('',#2775,#2774,#15,.T.);
#3381=EDGE_CURVE('',#2770,#2775,#16,.T.);
#3382=EDGE_CURVE('',#2776,#2774,#1736,.T.);
#3383=EDGE_CURVE('',#2776,#2777,#1737,.T.);
#3384=EDGE_CURVE('',#2777,#2775,#1738,.T.);
#3385=EDGE_CURVE('',#2778,#2773,#1739,.T.);
#3386=EDGE_CURVE('',#2778,#2776,#1740,.T.);
#3387=EDGE_CURVE('',#2779,#2772,#1741,.T.);
#3388=EDGE_CURVE('',#2779,#2778,#1742,.T.);
#3389=EDGE_CURVE('',#2780,#2771,#1743,.T.);
#3390=EDGE_CURVE('',#2780,#2779,#1744,.T.);
#3391=EDGE_CURVE('',#2781,#2770,#1745,.T.);
#3392=EDGE_CURVE('',#2781,#2780,#1746,.T.);
#3393=EDGE_CURVE('',#2777,#2781,#1747,.T.);
#3394=EDGE_CURVE('',#2782,#2783,#17,.T.);
#3395=EDGE_CURVE('',#2784,#2782,#18,.T.);
#3396=EDGE_CURVE('',#2784,#2785,#1748,.T.);
#3397=EDGE_CURVE('',#2785,#2785,#2364,.T.);
#3398=EDGE_CURVE('',#2786,#2784,#19,.T.);
#3399=EDGE_CURVE('',#2787,#2786,#20,.T.);
#3400=EDGE_CURVE('',#2788,#2787,#21,.T.);
#3401=EDGE_CURVE('',#2783,#2788,#22,.T.);
#3402=EDGE_CURVE('',#2789,#2789,#2365,.T.);
#3403=EDGE_CURVE('',#2789,#2790,#1749,.T.);
#3404=EDGE_CURVE('',#2791,#2790,#23,.T.);
#3405=EDGE_CURVE('',#2792,#2791,#24,.T.);
#3406=EDGE_CURVE('',#2793,#2792,#25,.T.);
#3407=EDGE_CURVE('',#2794,#2793,#26,.T.);
#3408=EDGE_CURVE('',#2795,#2794,#27,.T.);
#3409=EDGE_CURVE('',#2790,#2795,#28,.T.);
#3410=EDGE_CURVE('',#2786,#2795,#1750,.T.);
#3411=EDGE_CURVE('',#2787,#2794,#1751,.T.);
#3412=EDGE_CURVE('',#2784,#2790,#1752,.T.);
#3413=EDGE_CURVE('',#2782,#2791,#1753,.T.);
#3414=EDGE_CURVE('',#2796,#2796,#2366,.F.);
#3415=EDGE_CURVE('',#2796,#2797,#1754,.T.);
#3416=EDGE_CURVE('',#2797,#2797,#2367,.F.);
#3417=EDGE_CURVE('',#2783,#2792,#1755,.T.);
#3418=EDGE_CURVE('',#2788,#2793,#1756,.T.);
#3419=EDGE_CURVE('',#2798,#2798,#2368,.T.);
#3420=EDGE_CURVE('',#2798,#2799,#1757,.T.);
#3421=EDGE_CURVE('',#2799,#2799,#2369,.T.);
#3422=EDGE_CURVE('',#2800,#2800,#2370,.T.);
#3423=EDGE_CURVE('',#2800,#2801,#1758,.T.);
#3424=EDGE_CURVE('',#2801,#2801,#2371,.T.);
#3425=EDGE_CURVE('',#2802,#2802,#2372,.T.);
#3426=EDGE_CURVE('',#2802,#2803,#1759,.T.);
#3427=EDGE_CURVE('',#2803,#2803,#2373,.T.);
#3428=EDGE_CURVE('',#2804,#2804,#2374,.T.);
#3429=EDGE_CURVE('',#2804,#2805,#1760,.T.);
#3430=EDGE_CURVE('',#2805,#2805,#2375,.T.);
#3431=EDGE_CURVE('',#2806,#2806,#2376,.T.);
#3432=EDGE_CURVE('',#2806,#2807,#1761,.T.);
#3433=EDGE_CURVE('',#2807,#2807,#2377,.T.);
#3434=EDGE_CURVE('',#2808,#2808,#2378,.T.);
#3435=EDGE_CURVE('',#2808,#2809,#1762,.T.);
#3436=EDGE_CURVE('',#2809,#2809,#2379,.T.);
#3437=EDGE_CURVE('',#2810,#2810,#2380,.T.);
#3438=EDGE_CURVE('',#2810,#2811,#1763,.T.);
#3439=EDGE_CURVE('',#2811,#2811,#2381,.T.);
#3440=EDGE_CURVE('',#2812,#2812,#2382,.T.);
#3441=EDGE_CURVE('',#2812,#2813,#1764,.T.);
#3442=EDGE_CURVE('',#2813,#2813,#2383,.T.);
#3443=EDGE_CURVE('',#2814,#2814,#2384,.T.);
#3444=EDGE_CURVE('',#2814,#2815,#1765,.T.);
#3445=EDGE_CURVE('',#2815,#2815,#2385,.T.);
#3446=EDGE_CURVE('',#2816,#2816,#2386,.T.);
#3447=EDGE_CURVE('',#2816,#2817,#1766,.T.);
#3448=EDGE_CURVE('',#2817,#2817,#2387,.T.);
#3449=EDGE_CURVE('',#2818,#2818,#2388,.T.);
#3450=EDGE_CURVE('',#2818,#2819,#1767,.T.);
#3451=EDGE_CURVE('',#2819,#2819,#2389,.T.);
#3452=EDGE_CURVE('',#2820,#2820,#2390,.T.);
#3453=EDGE_CURVE('',#2820,#2821,#1768,.T.);
#3454=EDGE_CURVE('',#2821,#2821,#2391,.T.);
#3455=EDGE_CURVE('',#2822,#2822,#2392,.T.);
#3456=EDGE_CURVE('',#2823,#2823,#2393,.T.);
#3457=EDGE_CURVE('',#2823,#2822,#1769,.T.);
#3458=EDGE_CURVE('',#2824,#2824,#2394,.T.);
#3459=EDGE_CURVE('',#2824,#2825,#1770,.T.);
#3460=EDGE_CURVE('',#2825,#2825,#2395,.T.);
#3461=EDGE_CURVE('',#2826,#2826,#2396,.T.);
#3462=EDGE_CURVE('',#2826,#2827,#1771,.T.);
#3463=EDGE_CURVE('',#2827,#2827,#2397,.T.);
#3464=EDGE_CURVE('',#2828,#2828,#2398,.T.);
#3465=EDGE_CURVE('',#2828,#2829,#1772,.T.);
#3466=EDGE_CURVE('',#2829,#2829,#2399,.T.);
#3467=EDGE_CURVE('',#2830,#2830,#2400,.T.);
#3468=EDGE_CURVE('',#2830,#2831,#1773,.T.);
#3469=EDGE_CURVE('',#2831,#2831,#2401,.T.);
#3470=EDGE_CURVE('',#2832,#2832,#2402,.T.);
#3471=EDGE_CURVE('',#2832,#2833,#1774,.T.);
#3472=EDGE_CURVE('',#2833,#2833,#2403,.T.);
#3473=EDGE_CURVE('',#2834,#2834,#2404,.T.);
#3474=EDGE_CURVE('',#2834,#2835,#1775,.T.);
#3475=EDGE_CURVE('',#2835,#2835,#2405,.T.);
#3476=EDGE_CURVE('',#2836,#2836,#2406,.T.);
#3477=EDGE_CURVE('',#2836,#2837,#1776,.T.);
#3478=EDGE_CURVE('',#2837,#2837,#2407,.T.);
#3479=EDGE_CURVE('',#2838,#2838,#2408,.T.);
#3480=EDGE_CURVE('',#2838,#2839,#1777,.T.);
#3481=EDGE_CURVE('',#2839,#2839,#2409,.T.);
#3482=EDGE_CURVE('',#2840,#2840,#2410,.T.);
#3483=EDGE_CURVE('',#2840,#2841,#1778,.T.);
#3484=EDGE_CURVE('',#2841,#2841,#2411,.T.);
#3485=EDGE_CURVE('',#2842,#2842,#2412,.T.);
#3486=EDGE_CURVE('',#2843,#2843,#2413,.T.);
#3487=EDGE_CURVE('',#2843,#2842,#1779,.T.);
#3488=EDGE_CURVE('',#2844,#2844,#2414,.T.);
#3489=EDGE_CURVE('',#2844,#2843,#1780,.T.);
#3490=EDGE_CURVE('',#2845,#2845,#2415,.T.);
#3491=EDGE_CURVE('',#2845,#2844,#1781,.T.);
#3492=EDGE_CURVE('',#2846,#2846,#2416,.T.);
#3493=EDGE_CURVE('',#2847,#2847,#2417,.F.);
#3494=EDGE_CURVE('',#2847,#2846,#1782,.T.);
#3495=EDGE_CURVE('',#2848,#2848,#2418,.F.);
#3496=EDGE_CURVE('',#2848,#2847,#1783,.T.);
#3497=EDGE_CURVE('',#2849,#2849,#2419,.T.);
#3498=EDGE_CURVE('',#2849,#2848,#1784,.T.);
#3499=EDGE_CURVE('',#2850,#2851,#1785,.T.);
#3500=EDGE_CURVE('',#2851,#2852,#1786,.T.);
#3501=EDGE_CURVE('',#2852,#2853,#1787,.T.);
#3502=EDGE_CURVE('',#2850,#2853,#1788,.T.);
#3503=EDGE_CURVE('',#2851,#2854,#1789,.T.);
#3504=EDGE_CURVE('',#2854,#2855,#1790,.T.);
#3505=EDGE_CURVE('',#2855,#2852,#1791,.T.);
#3506=EDGE_CURVE('',#2854,#2856,#1792,.T.);
#3507=EDGE_CURVE('',#2856,#2857,#1793,.T.);
#3508=EDGE_CURVE('',#2857,#2855,#1794,.T.);
#3509=EDGE_CURVE('',#2856,#2858,#1795,.T.);
#3510=EDGE_CURVE('',#2858,#2859,#1796,.T.);
#3511=EDGE_CURVE('',#2859,#2857,#1797,.T.);
#3512=EDGE_CURVE('',#2858,#2860,#1798,.T.);
#3513=EDGE_CURVE('',#2860,#2861,#1799,.T.);
#3514=EDGE_CURVE('',#2861,#2859,#1800,.T.);
#3515=EDGE_CURVE('',#2860,#2850,#1801,.T.);
#3516=EDGE_CURVE('',#2853,#2861,#1802,.T.);
#3517=ORIENTED_EDGE('',*,*,#2862,.F.);
#3518=ORIENTED_EDGE('',*,*,#2863,.T.);
#3519=ORIENTED_EDGE('',*,*,#2864,.F.);
#3520=ORIENTED_EDGE('',*,*,#2863,.F.);
#3521=ORIENTED_EDGE('',*,*,#2862,.T.);
#3522=ORIENTED_EDGE('',*,*,#2865,.F.);
#3523=ORIENTED_EDGE('',*,*,#2866,.T.);
#3524=ORIENTED_EDGE('',*,*,#2867,.T.);
#3525=ORIENTED_EDGE('',*,*,#2866,.F.);
#3526=ORIENTED_EDGE('',*,*,#2867,.F.);
#3527=ORIENTED_EDGE('',*,*,#2868,.T.);
#3528=ORIENTED_EDGE('',*,*,#2869,.F.);
#3529=ORIENTED_EDGE('',*,*,#2870,.F.);
#3530=ORIENTED_EDGE('',*,*,#2871,.F.);
#3531=ORIENTED_EDGE('',*,*,#2868,.F.);
#3532=ORIENTED_EDGE('',*,*,#2872,.T.);
#3533=ORIENTED_EDGE('',*,*,#2870,.T.);
#3534=ORIENTED_EDGE('',*,*,#2872,.F.);
#3535=ORIENTED_EDGE('',*,*,#2871,.T.);
#3536=ORIENTED_EDGE('',*,*,#2873,.T.);
#3537=ORIENTED_EDGE('',*,*,#2874,.T.);
#3538=ORIENTED_EDGE('',*,*,#2873,.F.);
#3539=ORIENTED_EDGE('',*,*,#2875,.F.);
#3540=ORIENTED_EDGE('',*,*,#2876,.T.);
#3541=ORIENTED_EDGE('',*,*,#2869,.T.);
#3542=ORIENTED_EDGE('',*,*,#2876,.F.);
#3543=ORIENTED_EDGE('',*,*,#2875,.T.);
#3544=ORIENTED_EDGE('',*,*,#2864,.T.);
#3545=ORIENTED_EDGE('',*,*,#2874,.F.);
#3546=ORIENTED_EDGE('',*,*,#2865,.T.);
#3547=ORIENTED_EDGE('',*,*,#2877,.F.);
#3548=ORIENTED_EDGE('',*,*,#2878,.T.);
#3549=ORIENTED_EDGE('',*,*,#2879,.T.);
#3550=ORIENTED_EDGE('',*,*,#2878,.F.);
#3551=ORIENTED_EDGE('',*,*,#2880,.F.);
#3552=ORIENTED_EDGE('',*,*,#2881,.T.);
#3553=ORIENTED_EDGE('',*,*,#2882,.T.);
#3554=ORIENTED_EDGE('',*,*,#2881,.F.);
#3555=ORIENTED_EDGE('',*,*,#2880,.T.);
#3556=ORIENTED_EDGE('',*,*,#2877,.T.);
#3557=ORIENTED_EDGE('',*,*,#2882,.F.);
#3558=ORIENTED_EDGE('',*,*,#2879,.F.);
#3559=ORIENTED_EDGE('',*,*,#2883,.F.);
#3560=ORIENTED_EDGE('',*,*,#2884,.T.);
#3561=ORIENTED_EDGE('',*,*,#2885,.T.);
#3562=ORIENTED_EDGE('',*,*,#2884,.F.);
#3563=ORIENTED_EDGE('',*,*,#2886,.F.);
#3564=ORIENTED_EDGE('',*,*,#2887,.T.);
#3565=ORIENTED_EDGE('',*,*,#2888,.T.);
#3566=ORIENTED_EDGE('',*,*,#2887,.F.);
#3567=ORIENTED_EDGE('',*,*,#2886,.T.);
#3568=ORIENTED_EDGE('',*,*,#2883,.T.);
#3569=ORIENTED_EDGE('',*,*,#2888,.F.);
#3570=ORIENTED_EDGE('',*,*,#2885,.F.);
#3571=ORIENTED_EDGE('',*,*,#2889,.F.);
#3572=ORIENTED_EDGE('',*,*,#2890,.T.);
#3573=ORIENTED_EDGE('',*,*,#2891,.T.);
#3574=ORIENTED_EDGE('',*,*,#2890,.F.);
#3575=ORIENTED_EDGE('',*,*,#2892,.F.);
#3576=ORIENTED_EDGE('',*,*,#2893,.T.);
#3577=ORIENTED_EDGE('',*,*,#2894,.T.);
#3578=ORIENTED_EDGE('',*,*,#2893,.F.);
#3579=ORIENTED_EDGE('',*,*,#2892,.T.);
#3580=ORIENTED_EDGE('',*,*,#2889,.T.);
#3581=ORIENTED_EDGE('',*,*,#2894,.F.);
#3582=ORIENTED_EDGE('',*,*,#2891,.F.);
#3583=ORIENTED_EDGE('',*,*,#2895,.F.);
#3584=ORIENTED_EDGE('',*,*,#2896,.T.);
#3585=ORIENTED_EDGE('',*,*,#2897,.T.);
#3586=ORIENTED_EDGE('',*,*,#2896,.F.);
#3587=ORIENTED_EDGE('',*,*,#2898,.F.);
#3588=ORIENTED_EDGE('',*,*,#2899,.T.);
#3589=ORIENTED_EDGE('',*,*,#2900,.T.);
#3590=ORIENTED_EDGE('',*,*,#2899,.F.);
#3591=ORIENTED_EDGE('',*,*,#2898,.T.);
#3592=ORIENTED_EDGE('',*,*,#2895,.T.);
#3593=ORIENTED_EDGE('',*,*,#2900,.F.);
#3594=ORIENTED_EDGE('',*,*,#2897,.F.);
#3595=ORIENTED_EDGE('',*,*,#2901,.F.);
#3596=ORIENTED_EDGE('',*,*,#2902,.F.);
#3597=ORIENTED_EDGE('',*,*,#2903,.T.);
#3598=ORIENTED_EDGE('',*,*,#2904,.F.);
#3599=ORIENTED_EDGE('',*,*,#2905,.F.);
#3600=ORIENTED_EDGE('',*,*,#2903,.F.);
#3601=ORIENTED_EDGE('',*,*,#2904,.T.);
#3602=ORIENTED_EDGE('',*,*,#2905,.T.);
#3603=ORIENTED_EDGE('',*,*,#2906,.T.);
#3604=ORIENTED_EDGE('',*,*,#2907,.T.);
#3605=ORIENTED_EDGE('',*,*,#2906,.F.);
#3606=ORIENTED_EDGE('',*,*,#2908,.T.);
#3607=ORIENTED_EDGE('',*,*,#2909,.T.);
#3608=ORIENTED_EDGE('',*,*,#2910,.F.);
#3609=ORIENTED_EDGE('',*,*,#2909,.F.);
#3610=ORIENTED_EDGE('',*,*,#2910,.T.);
#3611=ORIENTED_EDGE('',*,*,#2911,.T.);
#3612=ORIENTED_EDGE('',*,*,#2912,.F.);
#3613=ORIENTED_EDGE('',*,*,#2911,.F.);
#3614=ORIENTED_EDGE('',*,*,#2907,.F.);
#3615=ORIENTED_EDGE('',*,*,#2912,.T.);
#3616=ORIENTED_EDGE('',*,*,#2913,.F.);
#3617=ORIENTED_EDGE('',*,*,#2914,.T.);
#3618=ORIENTED_EDGE('',*,*,#2901,.T.);
#3619=ORIENTED_EDGE('',*,*,#2902,.T.);
#3620=ORIENTED_EDGE('',*,*,#2914,.F.);
#3621=ORIENTED_EDGE('',*,*,#2913,.T.);
#3622=ORIENTED_EDGE('',*,*,#2915,.F.);
#3623=ORIENTED_EDGE('',*,*,#2915,.T.);
#3624=ORIENTED_EDGE('',*,*,#2916,.T.);
#3625=ORIENTED_EDGE('',*,*,#2908,.F.);
#3626=ORIENTED_EDGE('',*,*,#2916,.F.);
#3627=ORIENTED_EDGE('',*,*,#2917,.F.);
#3628=ORIENTED_EDGE('',*,*,#2918,.F.);
#3629=ORIENTED_EDGE('',*,*,#2919,.T.);
#3630=ORIENTED_EDGE('',*,*,#2920,.F.);
#3631=ORIENTED_EDGE('',*,*,#2921,.F.);
#3632=ORIENTED_EDGE('',*,*,#2919,.F.);
#3633=ORIENTED_EDGE('',*,*,#2922,.T.);
#3634=ORIENTED_EDGE('',*,*,#2923,.T.);
#3635=ORIENTED_EDGE('',*,*,#2920,.T.);
#3636=ORIENTED_EDGE('',*,*,#2921,.T.);
#3637=ORIENTED_EDGE('',*,*,#2923,.F.);
#3638=ORIENTED_EDGE('',*,*,#2924,.F.);
#3639=ORIENTED_EDGE('',*,*,#2925,.T.);
#3640=ORIENTED_EDGE('',*,*,#2926,.F.);
#3641=ORIENTED_EDGE('',*,*,#2927,.T.);
#3642=ORIENTED_EDGE('',*,*,#2924,.T.);
#3643=ORIENTED_EDGE('',*,*,#2927,.F.);
#3644=ORIENTED_EDGE('',*,*,#2928,.F.);
#3645=ORIENTED_EDGE('',*,*,#2929,.T.);
#3646=ORIENTED_EDGE('',*,*,#2926,.T.);
#3647=ORIENTED_EDGE('',*,*,#2929,.F.);
#3648=ORIENTED_EDGE('',*,*,#2930,.F.);
#3649=ORIENTED_EDGE('',*,*,#2931,.T.);
#3650=ORIENTED_EDGE('',*,*,#2928,.T.);
#3651=ORIENTED_EDGE('',*,*,#2931,.F.);
#3652=ORIENTED_EDGE('',*,*,#2930,.T.);
#3653=ORIENTED_EDGE('',*,*,#2922,.F.);
#3654=ORIENTED_EDGE('',*,*,#2917,.T.);
#3655=ORIENTED_EDGE('',*,*,#2918,.T.);
#3656=ORIENTED_EDGE('',*,*,#2932,.T.);
#3657=ORIENTED_EDGE('',*,*,#2925,.F.);
#3658=ORIENTED_EDGE('',*,*,#2932,.F.);
#3659=ORIENTED_EDGE('',*,*,#2933,.T.);
#3660=ORIENTED_EDGE('',*,*,#2933,.F.);
#3661=ORIENTED_EDGE('',*,*,#2934,.T.);
#3662=ORIENTED_EDGE('',*,*,#2934,.F.);
#3663=ORIENTED_EDGE('',*,*,#2935,.T.);
#3664=ORIENTED_EDGE('',*,*,#2935,.F.);
#3665=ORIENTED_EDGE('',*,*,#2936,.T.);
#3666=ORIENTED_EDGE('',*,*,#2936,.F.);
#3667=ORIENTED_EDGE('',*,*,#2937,.T.);
#3668=ORIENTED_EDGE('',*,*,#2937,.F.);
#3669=ORIENTED_EDGE('',*,*,#2938,.T.);
#3670=ORIENTED_EDGE('',*,*,#2938,.F.);
#3671=ORIENTED_EDGE('',*,*,#2939,.T.);
#3672=ORIENTED_EDGE('',*,*,#2939,.F.);
#3673=ORIENTED_EDGE('',*,*,#2940,.T.);
#3674=ORIENTED_EDGE('',*,*,#2940,.F.);
#3675=ORIENTED_EDGE('',*,*,#2941,.F.);
#3676=ORIENTED_EDGE('',*,*,#2942,.F.);
#3677=ORIENTED_EDGE('',*,*,#2943,.F.);
#3678=ORIENTED_EDGE('',*,*,#2944,.F.);
#3679=ORIENTED_EDGE('',*,*,#2943,.T.);
#3680=ORIENTED_EDGE('',*,*,#2945,.F.);
#3681=ORIENTED_EDGE('',*,*,#2946,.T.);
#3682=ORIENTED_EDGE('',*,*,#2947,.F.);
#3683=ORIENTED_EDGE('',*,*,#2948,.T.);
#3684=ORIENTED_EDGE('',*,*,#2949,.F.);
#3685=ORIENTED_EDGE('',*,*,#2950,.T.);
#3686=ORIENTED_EDGE('',*,*,#2951,.T.);
#3687=ORIENTED_EDGE('',*,*,#2952,.F.);
#3688=ORIENTED_EDGE('',*,*,#2951,.F.);
#3689=ORIENTED_EDGE('',*,*,#2953,.T.);
#3690=ORIENTED_EDGE('',*,*,#2954,.F.);
#3691=ORIENTED_EDGE('',*,*,#2955,.T.);
#3692=ORIENTED_EDGE('',*,*,#2956,.F.);
#3693=ORIENTED_EDGE('',*,*,#2957,.T.);
#3694=ORIENTED_EDGE('',*,*,#2958,.F.);
#3695=ORIENTED_EDGE('',*,*,#2959,.T.);
#3696=ORIENTED_EDGE('',*,*,#2960,.F.);
#3697=ORIENTED_EDGE('',*,*,#2961,.T.);
#3698=ORIENTED_EDGE('',*,*,#2962,.F.);
#3699=ORIENTED_EDGE('',*,*,#2942,.T.);
#3700=ORIENTED_EDGE('',*,*,#2963,.T.);
#3701=ORIENTED_EDGE('',*,*,#2964,.T.);
#3702=ORIENTED_EDGE('',*,*,#2945,.T.);
#3703=ORIENTED_EDGE('',*,*,#2965,.F.);
#3704=ORIENTED_EDGE('',*,*,#2966,.F.);
#3705=ORIENTED_EDGE('',*,*,#2946,.F.);
#3706=ORIENTED_EDGE('',*,*,#2964,.F.);
#3707=ORIENTED_EDGE('',*,*,#2966,.T.);
#3708=ORIENTED_EDGE('',*,*,#2967,.T.);
#3709=ORIENTED_EDGE('',*,*,#2968,.T.);
#3710=ORIENTED_EDGE('',*,*,#2947,.T.);
#3711=ORIENTED_EDGE('',*,*,#2969,.F.);
#3712=ORIENTED_EDGE('',*,*,#2970,.F.);
#3713=ORIENTED_EDGE('',*,*,#2948,.F.);
#3714=ORIENTED_EDGE('',*,*,#2968,.F.);
#3715=ORIENTED_EDGE('',*,*,#2970,.T.);
#3716=ORIENTED_EDGE('',*,*,#2971,.T.);
#3717=ORIENTED_EDGE('',*,*,#2972,.T.);
#3718=ORIENTED_EDGE('',*,*,#2949,.T.);
#3719=ORIENTED_EDGE('',*,*,#2973,.F.);
#3720=ORIENTED_EDGE('',*,*,#2974,.F.);
#3721=ORIENTED_EDGE('',*,*,#2953,.F.);
#3722=ORIENTED_EDGE('',*,*,#2950,.F.);
#3723=ORIENTED_EDGE('',*,*,#2972,.F.);
#3724=ORIENTED_EDGE('',*,*,#2975,.F.);
#3725=ORIENTED_EDGE('',*,*,#2974,.T.);
#3726=ORIENTED_EDGE('',*,*,#2976,.T.);
#3727=ORIENTED_EDGE('',*,*,#2977,.T.);
#3728=ORIENTED_EDGE('',*,*,#2954,.T.);
#3729=ORIENTED_EDGE('',*,*,#2978,.F.);
#3730=ORIENTED_EDGE('',*,*,#2979,.F.);
#3731=ORIENTED_EDGE('',*,*,#2955,.F.);
#3732=ORIENTED_EDGE('',*,*,#2977,.F.);
#3733=ORIENTED_EDGE('',*,*,#2979,.T.);
#3734=ORIENTED_EDGE('',*,*,#2980,.T.);
#3735=ORIENTED_EDGE('',*,*,#2981,.T.);
#3736=ORIENTED_EDGE('',*,*,#2956,.T.);
#3737=ORIENTED_EDGE('',*,*,#2982,.F.);
#3738=ORIENTED_EDGE('',*,*,#2983,.F.);
#3739=ORIENTED_EDGE('',*,*,#2957,.F.);
#3740=ORIENTED_EDGE('',*,*,#2981,.F.);
#3741=ORIENTED_EDGE('',*,*,#2983,.T.);
#3742=ORIENTED_EDGE('',*,*,#2984,.T.);
#3743=ORIENTED_EDGE('',*,*,#2985,.T.);
#3744=ORIENTED_EDGE('',*,*,#2958,.T.);
#3745=ORIENTED_EDGE('',*,*,#2959,.F.);
#3746=ORIENTED_EDGE('',*,*,#2985,.F.);
#3747=ORIENTED_EDGE('',*,*,#2986,.F.);
#3748=ORIENTED_EDGE('',*,*,#2987,.F.);
#3749=ORIENTED_EDGE('',*,*,#2988,.F.);
#3750=ORIENTED_EDGE('',*,*,#2989,.T.);
#3751=ORIENTED_EDGE('',*,*,#2975,.T.);
#3752=ORIENTED_EDGE('',*,*,#2971,.F.);
#3753=ORIENTED_EDGE('',*,*,#2969,.T.);
#3754=ORIENTED_EDGE('',*,*,#2967,.F.);
#3755=ORIENTED_EDGE('',*,*,#2965,.T.);
#3756=ORIENTED_EDGE('',*,*,#2963,.F.);
#3757=ORIENTED_EDGE('',*,*,#2941,.T.);
#3758=ORIENTED_EDGE('',*,*,#2990,.F.);
#3759=ORIENTED_EDGE('',*,*,#2991,.T.);
#3760=ORIENTED_EDGE('',*,*,#2992,.F.);
#3761=ORIENTED_EDGE('',*,*,#2986,.T.);
#3762=ORIENTED_EDGE('',*,*,#2984,.F.);
#3763=ORIENTED_EDGE('',*,*,#2982,.T.);
#3764=ORIENTED_EDGE('',*,*,#2980,.F.);
#3765=ORIENTED_EDGE('',*,*,#2978,.T.);
#3766=ORIENTED_EDGE('',*,*,#2976,.F.);
#3767=ORIENTED_EDGE('',*,*,#2973,.T.);
#3768=ORIENTED_EDGE('',*,*,#2989,.F.);
#3769=ORIENTED_EDGE('',*,*,#2944,.T.);
#3770=ORIENTED_EDGE('',*,*,#2962,.T.);
#3771=ORIENTED_EDGE('',*,*,#2993,.T.);
#3772=ORIENTED_EDGE('',*,*,#2990,.T.);
#3773=ORIENTED_EDGE('',*,*,#2961,.F.);
#3774=ORIENTED_EDGE('',*,*,#2994,.F.);
#3775=ORIENTED_EDGE('',*,*,#2991,.F.);
#3776=ORIENTED_EDGE('',*,*,#2993,.F.);
#3777=ORIENTED_EDGE('',*,*,#2952,.T.);
#3778=ORIENTED_EDGE('',*,*,#2988,.T.);
#3779=ORIENTED_EDGE('',*,*,#2987,.T.);
#3780=ORIENTED_EDGE('',*,*,#2992,.T.);
#3781=ORIENTED_EDGE('',*,*,#2994,.T.);
#3782=ORIENTED_EDGE('',*,*,#2960,.T.);
#3783=ORIENTED_EDGE('',*,*,#2995,.F.);
#3784=ORIENTED_EDGE('',*,*,#2996,.T.);
#3785=ORIENTED_EDGE('',*,*,#2997,.F.);
#3786=ORIENTED_EDGE('',*,*,#2998,.T.);
#3787=ORIENTED_EDGE('',*,*,#2995,.T.);
#3788=ORIENTED_EDGE('',*,*,#2998,.F.);
#3789=ORIENTED_EDGE('',*,*,#2997,.T.);
#3790=ORIENTED_EDGE('',*,*,#2999,.F.);
#3791=ORIENTED_EDGE('',*,*,#2999,.T.);
#3792=ORIENTED_EDGE('',*,*,#3000,.T.);
#3793=ORIENTED_EDGE('',*,*,#2996,.F.);
#3794=ORIENTED_EDGE('',*,*,#3000,.F.);
#3795=ORIENTED_EDGE('',*,*,#3001,.F.);
#3796=ORIENTED_EDGE('',*,*,#3002,.T.);
#3797=ORIENTED_EDGE('',*,*,#3003,.F.);
#3798=ORIENTED_EDGE('',*,*,#3004,.T.);
#3799=ORIENTED_EDGE('',*,*,#3001,.T.);
#3800=ORIENTED_EDGE('',*,*,#3004,.F.);
#3801=ORIENTED_EDGE('',*,*,#3003,.T.);
#3802=ORIENTED_EDGE('',*,*,#3005,.F.);
#3803=ORIENTED_EDGE('',*,*,#3005,.T.);
#3804=ORIENTED_EDGE('',*,*,#3006,.T.);
#3805=ORIENTED_EDGE('',*,*,#3002,.F.);
#3806=ORIENTED_EDGE('',*,*,#3006,.F.);
#3807=ORIENTED_EDGE('',*,*,#3007,.F.);
#3808=ORIENTED_EDGE('',*,*,#3008,.F.);
#3809=ORIENTED_EDGE('',*,*,#3009,.F.);
#3810=ORIENTED_EDGE('',*,*,#3010,.F.);
#3811=ORIENTED_EDGE('',*,*,#3011,.F.);
#3812=ORIENTED_EDGE('',*,*,#3012,.F.);
#3813=ORIENTED_EDGE('',*,*,#3013,.F.);
#3814=ORIENTED_EDGE('',*,*,#3014,.F.);
#3815=ORIENTED_EDGE('',*,*,#3007,.T.);
#3816=ORIENTED_EDGE('',*,*,#3015,.F.);
#3817=ORIENTED_EDGE('',*,*,#3016,.T.);
#3818=ORIENTED_EDGE('',*,*,#3017,.T.);
#3819=ORIENTED_EDGE('',*,*,#3011,.T.);
#3820=ORIENTED_EDGE('',*,*,#3018,.T.);
#3821=ORIENTED_EDGE('',*,*,#3019,.T.);
#3822=ORIENTED_EDGE('',*,*,#3020,.F.);
#3823=ORIENTED_EDGE('',*,*,#3021,.T.);
#3824=ORIENTED_EDGE('',*,*,#3008,.T.);
#3825=ORIENTED_EDGE('',*,*,#3017,.F.);
#3826=ORIENTED_EDGE('',*,*,#3022,.T.);
#3827=ORIENTED_EDGE('',*,*,#3023,.F.);
#3828=ORIENTED_EDGE('',*,*,#3014,.T.);
#3829=ORIENTED_EDGE('',*,*,#3024,.F.);
#3830=ORIENTED_EDGE('',*,*,#3025,.T.);
#3831=ORIENTED_EDGE('',*,*,#3018,.F.);
#3832=ORIENTED_EDGE('',*,*,#3009,.T.);
#3833=ORIENTED_EDGE('',*,*,#3023,.T.);
#3834=ORIENTED_EDGE('',*,*,#3026,.T.);
#3835=ORIENTED_EDGE('',*,*,#3027,.F.);
#3836=ORIENTED_EDGE('',*,*,#3013,.T.);
#3837=ORIENTED_EDGE('',*,*,#3028,.F.);
#3838=ORIENTED_EDGE('',*,*,#3029,.T.);
#3839=ORIENTED_EDGE('',*,*,#3024,.T.);
#3840=ORIENTED_EDGE('',*,*,#3030,.T.);
#3841=ORIENTED_EDGE('',*,*,#3031,.F.);
#3842=ORIENTED_EDGE('',*,*,#3032,.T.);
#3843=ORIENTED_EDGE('',*,*,#3033,.T.);
#3844=ORIENTED_EDGE('',*,*,#3032,.F.);
#3845=ORIENTED_EDGE('',*,*,#3034,.F.);
#3846=ORIENTED_EDGE('',*,*,#3035,.F.);
#3847=ORIENTED_EDGE('',*,*,#3036,.F.);
#3848=ORIENTED_EDGE('',*,*,#3037,.F.);
#3849=ORIENTED_EDGE('',*,*,#3029,.F.);
#3850=ORIENTED_EDGE('',*,*,#3038,.F.);
#3851=ORIENTED_EDGE('',*,*,#3019,.F.);
#3852=ORIENTED_EDGE('',*,*,#3025,.F.);
#3853=ORIENTED_EDGE('',*,*,#3034,.T.);
#3854=ORIENTED_EDGE('',*,*,#3039,.F.);
#3855=ORIENTED_EDGE('',*,*,#3040,.T.);
#3856=ORIENTED_EDGE('',*,*,#3041,.T.);
#3857=ORIENTED_EDGE('',*,*,#3035,.T.);
#3858=ORIENTED_EDGE('',*,*,#3041,.F.);
#3859=ORIENTED_EDGE('',*,*,#3042,.F.);
#3860=ORIENTED_EDGE('',*,*,#3043,.F.);
#3861=ORIENTED_EDGE('',*,*,#3036,.T.);
#3862=ORIENTED_EDGE('',*,*,#3043,.T.);
#3863=ORIENTED_EDGE('',*,*,#3044,.T.);
#3864=ORIENTED_EDGE('',*,*,#3045,.F.);
#3865=ORIENTED_EDGE('',*,*,#3046,.F.);
#3866=ORIENTED_EDGE('',*,*,#3047,.T.);
#3867=ORIENTED_EDGE('',*,*,#3048,.T.);
#3868=ORIENTED_EDGE('',*,*,#3047,.F.);
#3869=ORIENTED_EDGE('',*,*,#3021,.F.);
#3870=ORIENTED_EDGE('',*,*,#3049,.T.);
#3871=ORIENTED_EDGE('',*,*,#3030,.F.);
#3872=ORIENTED_EDGE('',*,*,#3049,.F.);
#3873=ORIENTED_EDGE('',*,*,#3050,.F.);
#3874=ORIENTED_EDGE('',*,*,#3026,.F.);
#3875=ORIENTED_EDGE('',*,*,#3022,.F.);
#3876=ORIENTED_EDGE('',*,*,#3016,.F.);
#3877=ORIENTED_EDGE('',*,*,#3051,.F.);
#3878=ORIENTED_EDGE('',*,*,#3044,.F.);
#3879=ORIENTED_EDGE('',*,*,#3042,.T.);
#3880=ORIENTED_EDGE('',*,*,#3040,.F.);
#3881=ORIENTED_EDGE('',*,*,#3052,.T.);
#3882=ORIENTED_EDGE('',*,*,#3053,.T.);
#3883=ORIENTED_EDGE('',*,*,#3054,.F.);
#3884=ORIENTED_EDGE('',*,*,#3055,.F.);
#3885=ORIENTED_EDGE('',*,*,#3056,.T.);
#3886=ORIENTED_EDGE('',*,*,#3055,.T.);
#3887=ORIENTED_EDGE('',*,*,#3057,.F.);
#3888=ORIENTED_EDGE('',*,*,#3058,.F.);
#3889=ORIENTED_EDGE('',*,*,#3059,.T.);
#3890=ORIENTED_EDGE('',*,*,#3058,.T.);
#3891=ORIENTED_EDGE('',*,*,#3060,.F.);
#3892=ORIENTED_EDGE('',*,*,#3061,.F.);
#3893=ORIENTED_EDGE('',*,*,#3062,.T.);
#3894=ORIENTED_EDGE('',*,*,#3061,.T.);
#3895=ORIENTED_EDGE('',*,*,#3063,.F.);
#3896=ORIENTED_EDGE('',*,*,#3053,.F.);
#3897=ORIENTED_EDGE('',*,*,#3063,.T.);
#3898=ORIENTED_EDGE('',*,*,#3060,.T.);
#3899=ORIENTED_EDGE('',*,*,#3057,.T.);
#3900=ORIENTED_EDGE('',*,*,#3054,.T.);
#3901=ORIENTED_EDGE('',*,*,#3020,.T.);
#3902=ORIENTED_EDGE('',*,*,#3038,.T.);
#3903=ORIENTED_EDGE('',*,*,#3028,.T.);
#3904=ORIENTED_EDGE('',*,*,#3012,.T.);
#3905=ORIENTED_EDGE('',*,*,#3033,.F.);
#3906=ORIENTED_EDGE('',*,*,#3010,.T.);
#3907=ORIENTED_EDGE('',*,*,#3027,.T.);
#3908=ORIENTED_EDGE('',*,*,#3050,.T.);
#3909=ORIENTED_EDGE('',*,*,#3015,.T.);
#3910=ORIENTED_EDGE('',*,*,#3048,.F.);
#3911=ORIENTED_EDGE('',*,*,#3037,.T.);
#3912=ORIENTED_EDGE('',*,*,#3045,.T.);
#3913=ORIENTED_EDGE('',*,*,#3051,.T.);
#3914=ORIENTED_EDGE('',*,*,#3039,.T.);
#3915=ORIENTED_EDGE('',*,*,#3062,.F.);
#3916=ORIENTED_EDGE('',*,*,#3052,.F.);
#3917=ORIENTED_EDGE('',*,*,#3056,.F.);
#3918=ORIENTED_EDGE('',*,*,#3059,.F.);
#3919=ORIENTED_EDGE('',*,*,#3031,.T.);
#3920=ORIENTED_EDGE('',*,*,#3046,.T.);
#3921=ORIENTED_EDGE('',*,*,#3064,.F.);
#3922=ORIENTED_EDGE('',*,*,#3065,.T.);
#3923=ORIENTED_EDGE('',*,*,#3066,.F.);
#3924=ORIENTED_EDGE('',*,*,#3065,.F.);
#3925=ORIENTED_EDGE('',*,*,#3067,.F.);
#3926=ORIENTED_EDGE('',*,*,#3068,.T.);
#3927=ORIENTED_EDGE('',*,*,#3069,.F.);
#3928=ORIENTED_EDGE('',*,*,#3068,.F.);
#3929=ORIENTED_EDGE('',*,*,#3070,.T.);
#3930=ORIENTED_EDGE('',*,*,#3071,.T.);
#3931=ORIENTED_EDGE('',*,*,#3072,.F.);
#3932=ORIENTED_EDGE('',*,*,#3073,.F.);
#3933=ORIENTED_EDGE('',*,*,#3074,.F.);
#3934=ORIENTED_EDGE('',*,*,#3075,.T.);
#3935=ORIENTED_EDGE('',*,*,#3072,.T.);
#3936=ORIENTED_EDGE('',*,*,#3076,.T.);
#3937=ORIENTED_EDGE('',*,*,#3069,.T.);
#3938=ORIENTED_EDGE('',*,*,#3074,.T.);
#3939=ORIENTED_EDGE('',*,*,#3077,.T.);
#3940=ORIENTED_EDGE('',*,*,#3078,.T.);
#3941=ORIENTED_EDGE('',*,*,#3079,.T.);
#3942=ORIENTED_EDGE('',*,*,#3066,.T.);
#3943=ORIENTED_EDGE('',*,*,#3080,.F.);
#3944=ORIENTED_EDGE('',*,*,#3081,.T.);
#3945=ORIENTED_EDGE('',*,*,#3082,.T.);
#3946=ORIENTED_EDGE('',*,*,#3077,.F.);
#3947=ORIENTED_EDGE('',*,*,#3076,.F.);
#3948=ORIENTED_EDGE('',*,*,#3071,.F.);
#3949=ORIENTED_EDGE('',*,*,#3079,.F.);
#3950=ORIENTED_EDGE('',*,*,#3083,.F.);
#3951=ORIENTED_EDGE('',*,*,#3084,.T.);
#3952=ORIENTED_EDGE('',*,*,#3085,.T.);
#3953=ORIENTED_EDGE('',*,*,#3073,.T.);
#3954=ORIENTED_EDGE('',*,*,#3075,.F.);
#3955=ORIENTED_EDGE('',*,*,#3086,.T.);
#3956=ORIENTED_EDGE('',*,*,#3083,.T.);
#3957=ORIENTED_EDGE('',*,*,#3078,.F.);
#3958=ORIENTED_EDGE('',*,*,#3082,.F.);
#3959=ORIENTED_EDGE('',*,*,#3085,.F.);
#3960=ORIENTED_EDGE('',*,*,#3087,.T.);
#3961=ORIENTED_EDGE('',*,*,#3080,.T.);
#3962=ORIENTED_EDGE('',*,*,#3070,.F.);
#3963=ORIENTED_EDGE('',*,*,#3067,.T.);
#3964=ORIENTED_EDGE('',*,*,#3087,.F.);
#3965=ORIENTED_EDGE('',*,*,#3084,.F.);
#3966=ORIENTED_EDGE('',*,*,#3086,.F.);
#3967=ORIENTED_EDGE('',*,*,#3081,.F.);
#3968=ORIENTED_EDGE('',*,*,#3064,.T.);
#3969=ORIENTED_EDGE('',*,*,#3088,.F.);
#3970=ORIENTED_EDGE('',*,*,#3089,.F.);
#3971=ORIENTED_EDGE('',*,*,#3090,.F.);
#3972=ORIENTED_EDGE('',*,*,#3091,.F.);
#3973=ORIENTED_EDGE('',*,*,#3092,.F.);
#3974=ORIENTED_EDGE('',*,*,#3093,.F.);
#3975=ORIENTED_EDGE('',*,*,#3094,.F.);
#3976=ORIENTED_EDGE('',*,*,#3095,.F.);
#3977=ORIENTED_EDGE('',*,*,#3088,.T.);
#3978=ORIENTED_EDGE('',*,*,#3096,.F.);
#3979=ORIENTED_EDGE('',*,*,#3097,.T.);
#3980=ORIENTED_EDGE('',*,*,#3098,.T.);
#3981=ORIENTED_EDGE('',*,*,#3092,.T.);
#3982=ORIENTED_EDGE('',*,*,#3099,.T.);
#3983=ORIENTED_EDGE('',*,*,#3100,.T.);
#3984=ORIENTED_EDGE('',*,*,#3101,.F.);
#3985=ORIENTED_EDGE('',*,*,#3102,.T.);
#3986=ORIENTED_EDGE('',*,*,#3089,.T.);
#3987=ORIENTED_EDGE('',*,*,#3098,.F.);
#3988=ORIENTED_EDGE('',*,*,#3103,.T.);
#3989=ORIENTED_EDGE('',*,*,#3104,.F.);
#3990=ORIENTED_EDGE('',*,*,#3095,.T.);
#3991=ORIENTED_EDGE('',*,*,#3105,.F.);
#3992=ORIENTED_EDGE('',*,*,#3106,.T.);
#3993=ORIENTED_EDGE('',*,*,#3099,.F.);
#3994=ORIENTED_EDGE('',*,*,#3090,.T.);
#3995=ORIENTED_EDGE('',*,*,#3104,.T.);
#3996=ORIENTED_EDGE('',*,*,#3107,.T.);
#3997=ORIENTED_EDGE('',*,*,#3108,.F.);
#3998=ORIENTED_EDGE('',*,*,#3094,.T.);
#3999=ORIENTED_EDGE('',*,*,#3109,.F.);
#4000=ORIENTED_EDGE('',*,*,#3110,.T.);
#4001=ORIENTED_EDGE('',*,*,#3105,.T.);
#4002=ORIENTED_EDGE('',*,*,#3111,.T.);
#4003=ORIENTED_EDGE('',*,*,#3112,.F.);
#4004=ORIENTED_EDGE('',*,*,#3113,.T.);
#4005=ORIENTED_EDGE('',*,*,#3114,.T.);
#4006=ORIENTED_EDGE('',*,*,#3113,.F.);
#4007=ORIENTED_EDGE('',*,*,#3115,.F.);
#4008=ORIENTED_EDGE('',*,*,#3116,.F.);
#4009=ORIENTED_EDGE('',*,*,#3117,.F.);
#4010=ORIENTED_EDGE('',*,*,#3118,.F.);
#4011=ORIENTED_EDGE('',*,*,#3110,.F.);
#4012=ORIENTED_EDGE('',*,*,#3119,.F.);
#4013=ORIENTED_EDGE('',*,*,#3100,.F.);
#4014=ORIENTED_EDGE('',*,*,#3106,.F.);
#4015=ORIENTED_EDGE('',*,*,#3115,.T.);
#4016=ORIENTED_EDGE('',*,*,#3120,.F.);
#4017=ORIENTED_EDGE('',*,*,#3121,.T.);
#4018=ORIENTED_EDGE('',*,*,#3122,.T.);
#4019=ORIENTED_EDGE('',*,*,#3116,.T.);
#4020=ORIENTED_EDGE('',*,*,#3122,.F.);
#4021=ORIENTED_EDGE('',*,*,#3123,.F.);
#4022=ORIENTED_EDGE('',*,*,#3124,.F.);
#4023=ORIENTED_EDGE('',*,*,#3117,.T.);
#4024=ORIENTED_EDGE('',*,*,#3124,.T.);
#4025=ORIENTED_EDGE('',*,*,#3125,.T.);
#4026=ORIENTED_EDGE('',*,*,#3126,.F.);
#4027=ORIENTED_EDGE('',*,*,#3127,.F.);
#4028=ORIENTED_EDGE('',*,*,#3128,.T.);
#4029=ORIENTED_EDGE('',*,*,#3129,.T.);
#4030=ORIENTED_EDGE('',*,*,#3128,.F.);
#4031=ORIENTED_EDGE('',*,*,#3102,.F.);
#4032=ORIENTED_EDGE('',*,*,#3130,.T.);
#4033=ORIENTED_EDGE('',*,*,#3111,.F.);
#4034=ORIENTED_EDGE('',*,*,#3130,.F.);
#4035=ORIENTED_EDGE('',*,*,#3131,.F.);
#4036=ORIENTED_EDGE('',*,*,#3107,.F.);
#4037=ORIENTED_EDGE('',*,*,#3103,.F.);
#4038=ORIENTED_EDGE('',*,*,#3097,.F.);
#4039=ORIENTED_EDGE('',*,*,#3132,.F.);
#4040=ORIENTED_EDGE('',*,*,#3125,.F.);
#4041=ORIENTED_EDGE('',*,*,#3123,.T.);
#4042=ORIENTED_EDGE('',*,*,#3121,.F.);
#4043=ORIENTED_EDGE('',*,*,#3133,.T.);
#4044=ORIENTED_EDGE('',*,*,#3134,.T.);
#4045=ORIENTED_EDGE('',*,*,#3135,.F.);
#4046=ORIENTED_EDGE('',*,*,#3136,.F.);
#4047=ORIENTED_EDGE('',*,*,#3137,.T.);
#4048=ORIENTED_EDGE('',*,*,#3136,.T.);
#4049=ORIENTED_EDGE('',*,*,#3138,.F.);
#4050=ORIENTED_EDGE('',*,*,#3139,.F.);
#4051=ORIENTED_EDGE('',*,*,#3140,.T.);
#4052=ORIENTED_EDGE('',*,*,#3139,.T.);
#4053=ORIENTED_EDGE('',*,*,#3141,.F.);
#4054=ORIENTED_EDGE('',*,*,#3142,.F.);
#4055=ORIENTED_EDGE('',*,*,#3143,.T.);
#4056=ORIENTED_EDGE('',*,*,#3142,.T.);
#4057=ORIENTED_EDGE('',*,*,#3144,.F.);
#4058=ORIENTED_EDGE('',*,*,#3134,.F.);
#4059=ORIENTED_EDGE('',*,*,#3144,.T.);
#4060=ORIENTED_EDGE('',*,*,#3141,.T.);
#4061=ORIENTED_EDGE('',*,*,#3138,.T.);
#4062=ORIENTED_EDGE('',*,*,#3135,.T.);
#4063=ORIENTED_EDGE('',*,*,#3101,.T.);
#4064=ORIENTED_EDGE('',*,*,#3119,.T.);
#4065=ORIENTED_EDGE('',*,*,#3109,.T.);
#4066=ORIENTED_EDGE('',*,*,#3093,.T.);
#4067=ORIENTED_EDGE('',*,*,#3114,.F.);
#4068=ORIENTED_EDGE('',*,*,#3091,.T.);
#4069=ORIENTED_EDGE('',*,*,#3108,.T.);
#4070=ORIENTED_EDGE('',*,*,#3131,.T.);
#4071=ORIENTED_EDGE('',*,*,#3096,.T.);
#4072=ORIENTED_EDGE('',*,*,#3129,.F.);
#4073=ORIENTED_EDGE('',*,*,#3118,.T.);
#4074=ORIENTED_EDGE('',*,*,#3126,.T.);
#4075=ORIENTED_EDGE('',*,*,#3132,.T.);
#4076=ORIENTED_EDGE('',*,*,#3120,.T.);
#4077=ORIENTED_EDGE('',*,*,#3143,.F.);
#4078=ORIENTED_EDGE('',*,*,#3133,.F.);
#4079=ORIENTED_EDGE('',*,*,#3137,.F.);
#4080=ORIENTED_EDGE('',*,*,#3140,.F.);
#4081=ORIENTED_EDGE('',*,*,#3112,.T.);
#4082=ORIENTED_EDGE('',*,*,#3127,.T.);
#4083=ORIENTED_EDGE('',*,*,#3145,.F.);
#4084=ORIENTED_EDGE('',*,*,#3146,.T.);
#4085=ORIENTED_EDGE('',*,*,#3147,.F.);
#4086=ORIENTED_EDGE('',*,*,#3146,.F.);
#4087=ORIENTED_EDGE('',*,*,#3148,.F.);
#4088=ORIENTED_EDGE('',*,*,#3149,.T.);
#4089=ORIENTED_EDGE('',*,*,#3150,.F.);
#4090=ORIENTED_EDGE('',*,*,#3149,.F.);
#4091=ORIENTED_EDGE('',*,*,#3151,.T.);
#4092=ORIENTED_EDGE('',*,*,#3152,.T.);
#4093=ORIENTED_EDGE('',*,*,#3153,.F.);
#4094=ORIENTED_EDGE('',*,*,#3154,.F.);
#4095=ORIENTED_EDGE('',*,*,#3155,.F.);
#4096=ORIENTED_EDGE('',*,*,#3156,.T.);
#4097=ORIENTED_EDGE('',*,*,#3153,.T.);
#4098=ORIENTED_EDGE('',*,*,#3157,.T.);
#4099=ORIENTED_EDGE('',*,*,#3150,.T.);
#4100=ORIENTED_EDGE('',*,*,#3155,.T.);
#4101=ORIENTED_EDGE('',*,*,#3158,.T.);
#4102=ORIENTED_EDGE('',*,*,#3159,.T.);
#4103=ORIENTED_EDGE('',*,*,#3160,.T.);
#4104=ORIENTED_EDGE('',*,*,#3147,.T.);
#4105=ORIENTED_EDGE('',*,*,#3161,.F.);
#4106=ORIENTED_EDGE('',*,*,#3162,.T.);
#4107=ORIENTED_EDGE('',*,*,#3163,.T.);
#4108=ORIENTED_EDGE('',*,*,#3158,.F.);
#4109=ORIENTED_EDGE('',*,*,#3157,.F.);
#4110=ORIENTED_EDGE('',*,*,#3152,.F.);
#4111=ORIENTED_EDGE('',*,*,#3160,.F.);
#4112=ORIENTED_EDGE('',*,*,#3164,.F.);
#4113=ORIENTED_EDGE('',*,*,#3165,.T.);
#4114=ORIENTED_EDGE('',*,*,#3166,.T.);
#4115=ORIENTED_EDGE('',*,*,#3154,.T.);
#4116=ORIENTED_EDGE('',*,*,#3156,.F.);
#4117=ORIENTED_EDGE('',*,*,#3167,.T.);
#4118=ORIENTED_EDGE('',*,*,#3164,.T.);
#4119=ORIENTED_EDGE('',*,*,#3159,.F.);
#4120=ORIENTED_EDGE('',*,*,#3163,.F.);
#4121=ORIENTED_EDGE('',*,*,#3166,.F.);
#4122=ORIENTED_EDGE('',*,*,#3168,.T.);
#4123=ORIENTED_EDGE('',*,*,#3161,.T.);
#4124=ORIENTED_EDGE('',*,*,#3151,.F.);
#4125=ORIENTED_EDGE('',*,*,#3148,.T.);
#4126=ORIENTED_EDGE('',*,*,#3168,.F.);
#4127=ORIENTED_EDGE('',*,*,#3165,.F.);
#4128=ORIENTED_EDGE('',*,*,#3167,.F.);
#4129=ORIENTED_EDGE('',*,*,#3162,.F.);
#4130=ORIENTED_EDGE('',*,*,#3145,.T.);
#4131=ORIENTED_EDGE('',*,*,#3169,.F.);
#4132=ORIENTED_EDGE('',*,*,#3170,.T.);
#4133=ORIENTED_EDGE('',*,*,#3171,.F.);
#4134=ORIENTED_EDGE('',*,*,#3172,.F.);
#4135=ORIENTED_EDGE('',*,*,#3173,.F.);
#4136=ORIENTED_EDGE('',*,*,#3174,.T.);
#4137=ORIENTED_EDGE('',*,*,#3175,.F.);
#4138=ORIENTED_EDGE('',*,*,#3170,.F.);
#4139=ORIENTED_EDGE('',*,*,#3176,.F.);
#4140=ORIENTED_EDGE('',*,*,#3177,.T.);
#4141=ORIENTED_EDGE('',*,*,#3178,.F.);
#4142=ORIENTED_EDGE('',*,*,#3174,.F.);
#4143=ORIENTED_EDGE('',*,*,#3179,.F.);
#4144=ORIENTED_EDGE('',*,*,#3180,.T.);
#4145=ORIENTED_EDGE('',*,*,#3181,.F.);
#4146=ORIENTED_EDGE('',*,*,#3177,.F.);
#4147=ORIENTED_EDGE('',*,*,#3182,.F.);
#4148=ORIENTED_EDGE('',*,*,#3183,.T.);
#4149=ORIENTED_EDGE('',*,*,#3184,.F.);
#4150=ORIENTED_EDGE('',*,*,#3180,.F.);
#4151=ORIENTED_EDGE('',*,*,#3185,.F.);
#4152=ORIENTED_EDGE('',*,*,#3186,.T.);
#4153=ORIENTED_EDGE('',*,*,#3187,.F.);
#4154=ORIENTED_EDGE('',*,*,#3183,.F.);
#4155=ORIENTED_EDGE('',*,*,#3188,.F.);
#4156=ORIENTED_EDGE('',*,*,#3189,.T.);
#4157=ORIENTED_EDGE('',*,*,#3190,.F.);
#4158=ORIENTED_EDGE('',*,*,#3186,.F.);
#4159=ORIENTED_EDGE('',*,*,#3191,.F.);
#4160=ORIENTED_EDGE('',*,*,#3192,.T.);
#4161=ORIENTED_EDGE('',*,*,#3193,.F.);
#4162=ORIENTED_EDGE('',*,*,#3189,.F.);
#4163=ORIENTED_EDGE('',*,*,#3194,.F.);
#4164=ORIENTED_EDGE('',*,*,#3195,.F.);
#4165=ORIENTED_EDGE('',*,*,#3196,.F.);
#4166=ORIENTED_EDGE('',*,*,#3192,.F.);
#4167=ORIENTED_EDGE('',*,*,#3197,.F.);
#4168=ORIENTED_EDGE('',*,*,#3198,.T.);
#4169=ORIENTED_EDGE('',*,*,#3199,.F.);
#4170=ORIENTED_EDGE('',*,*,#3200,.F.);
#4171=ORIENTED_EDGE('',*,*,#3201,.F.);
#4172=ORIENTED_EDGE('',*,*,#3202,.T.);
#4173=ORIENTED_EDGE('',*,*,#3203,.F.);
#4174=ORIENTED_EDGE('',*,*,#3198,.F.);
#4175=ORIENTED_EDGE('',*,*,#3204,.F.);
#4176=ORIENTED_EDGE('',*,*,#3205,.T.);
#4177=ORIENTED_EDGE('',*,*,#3206,.F.);
#4178=ORIENTED_EDGE('',*,*,#3202,.F.);
#4179=ORIENTED_EDGE('',*,*,#3207,.F.);
#4180=ORIENTED_EDGE('',*,*,#3208,.T.);
#4181=ORIENTED_EDGE('',*,*,#3209,.F.);
#4182=ORIENTED_EDGE('',*,*,#3205,.F.);
#4183=ORIENTED_EDGE('',*,*,#3210,.F.);
#4184=ORIENTED_EDGE('',*,*,#3211,.T.);
#4185=ORIENTED_EDGE('',*,*,#3212,.F.);
#4186=ORIENTED_EDGE('',*,*,#3208,.F.);
#4187=ORIENTED_EDGE('',*,*,#3213,.F.);
#4188=ORIENTED_EDGE('',*,*,#3214,.T.);
#4189=ORIENTED_EDGE('',*,*,#3215,.F.);
#4190=ORIENTED_EDGE('',*,*,#3211,.F.);
#4191=ORIENTED_EDGE('',*,*,#3216,.F.);
#4192=ORIENTED_EDGE('',*,*,#3217,.T.);
#4193=ORIENTED_EDGE('',*,*,#3218,.F.);
#4194=ORIENTED_EDGE('',*,*,#3214,.F.);
#4195=ORIENTED_EDGE('',*,*,#3219,.F.);
#4196=ORIENTED_EDGE('',*,*,#3220,.T.);
#4197=ORIENTED_EDGE('',*,*,#3221,.F.);
#4198=ORIENTED_EDGE('',*,*,#3217,.F.);
#4199=ORIENTED_EDGE('',*,*,#3222,.F.);
#4200=ORIENTED_EDGE('',*,*,#3223,.F.);
#4201=ORIENTED_EDGE('',*,*,#3224,.F.);
#4202=ORIENTED_EDGE('',*,*,#3220,.F.);
#4203=ORIENTED_EDGE('',*,*,#3225,.F.);
#4204=ORIENTED_EDGE('',*,*,#3226,.T.);
#4205=ORIENTED_EDGE('',*,*,#3227,.F.);
#4206=ORIENTED_EDGE('',*,*,#3228,.F.);
#4207=ORIENTED_EDGE('',*,*,#3229,.F.);
#4208=ORIENTED_EDGE('',*,*,#3230,.T.);
#4209=ORIENTED_EDGE('',*,*,#3231,.F.);
#4210=ORIENTED_EDGE('',*,*,#3226,.F.);
#4211=ORIENTED_EDGE('',*,*,#3232,.F.);
#4212=ORIENTED_EDGE('',*,*,#3233,.T.);
#4213=ORIENTED_EDGE('',*,*,#3234,.F.);
#4214=ORIENTED_EDGE('',*,*,#3230,.F.);
#4215=ORIENTED_EDGE('',*,*,#3235,.F.);
#4216=ORIENTED_EDGE('',*,*,#3236,.T.);
#4217=ORIENTED_EDGE('',*,*,#3237,.F.);
#4218=ORIENTED_EDGE('',*,*,#3233,.F.);
#4219=ORIENTED_EDGE('',*,*,#3238,.F.);
#4220=ORIENTED_EDGE('',*,*,#3239,.T.);
#4221=ORIENTED_EDGE('',*,*,#3240,.F.);
#4222=ORIENTED_EDGE('',*,*,#3236,.F.);
#4223=ORIENTED_EDGE('',*,*,#3241,.F.);
#4224=ORIENTED_EDGE('',*,*,#3242,.T.);
#4225=ORIENTED_EDGE('',*,*,#3243,.F.);
#4226=ORIENTED_EDGE('',*,*,#3239,.F.);
#4227=ORIENTED_EDGE('',*,*,#3244,.F.);
#4228=ORIENTED_EDGE('',*,*,#3245,.T.);
#4229=ORIENTED_EDGE('',*,*,#3246,.F.);
#4230=ORIENTED_EDGE('',*,*,#3242,.F.);
#4231=ORIENTED_EDGE('',*,*,#3247,.F.);
#4232=ORIENTED_EDGE('',*,*,#3248,.T.);
#4233=ORIENTED_EDGE('',*,*,#3249,.F.);
#4234=ORIENTED_EDGE('',*,*,#3245,.F.);
#4235=ORIENTED_EDGE('',*,*,#3250,.F.);
#4236=ORIENTED_EDGE('',*,*,#3251,.F.);
#4237=ORIENTED_EDGE('',*,*,#3252,.F.);
#4238=ORIENTED_EDGE('',*,*,#3248,.F.);
#4239=ORIENTED_EDGE('',*,*,#3253,.F.);
#4240=ORIENTED_EDGE('',*,*,#3254,.T.);
#4241=ORIENTED_EDGE('',*,*,#3255,.F.);
#4242=ORIENTED_EDGE('',*,*,#3256,.F.);
#4243=ORIENTED_EDGE('',*,*,#3257,.F.);
#4244=ORIENTED_EDGE('',*,*,#3258,.T.);
#4245=ORIENTED_EDGE('',*,*,#3259,.F.);
#4246=ORIENTED_EDGE('',*,*,#3254,.F.);
#4247=ORIENTED_EDGE('',*,*,#3260,.F.);
#4248=ORIENTED_EDGE('',*,*,#3261,.T.);
#4249=ORIENTED_EDGE('',*,*,#3262,.F.);
#4250=ORIENTED_EDGE('',*,*,#3258,.F.);
#4251=ORIENTED_EDGE('',*,*,#3263,.F.);
#4252=ORIENTED_EDGE('',*,*,#3264,.T.);
#4253=ORIENTED_EDGE('',*,*,#3265,.F.);
#4254=ORIENTED_EDGE('',*,*,#3261,.F.);
#4255=ORIENTED_EDGE('',*,*,#3266,.F.);
#4256=ORIENTED_EDGE('',*,*,#3267,.T.);
#4257=ORIENTED_EDGE('',*,*,#3268,.F.);
#4258=ORIENTED_EDGE('',*,*,#3264,.F.);
#4259=ORIENTED_EDGE('',*,*,#3269,.F.);
#4260=ORIENTED_EDGE('',*,*,#3270,.T.);
#4261=ORIENTED_EDGE('',*,*,#3271,.F.);
#4262=ORIENTED_EDGE('',*,*,#3267,.F.);
#4263=ORIENTED_EDGE('',*,*,#3272,.F.);
#4264=ORIENTED_EDGE('',*,*,#3273,.T.);
#4265=ORIENTED_EDGE('',*,*,#3274,.F.);
#4266=ORIENTED_EDGE('',*,*,#3270,.F.);
#4267=ORIENTED_EDGE('',*,*,#3275,.F.);
#4268=ORIENTED_EDGE('',*,*,#3276,.T.);
#4269=ORIENTED_EDGE('',*,*,#3277,.F.);
#4270=ORIENTED_EDGE('',*,*,#3273,.F.);
#4271=ORIENTED_EDGE('',*,*,#3278,.F.);
#4272=ORIENTED_EDGE('',*,*,#3279,.F.);
#4273=ORIENTED_EDGE('',*,*,#3280,.F.);
#4274=ORIENTED_EDGE('',*,*,#3276,.F.);
#4275=ORIENTED_EDGE('',*,*,#3281,.F.);
#4276=ORIENTED_EDGE('',*,*,#3282,.T.);
#4277=ORIENTED_EDGE('',*,*,#3283,.F.);
#4278=ORIENTED_EDGE('',*,*,#3282,.F.);
#4279=ORIENTED_EDGE('',*,*,#3195,.T.);
#4280=ORIENTED_EDGE('',*,*,#3284,.T.);
#4281=ORIENTED_EDGE('',*,*,#3285,.T.);
#4282=ORIENTED_EDGE('',*,*,#3286,.F.);
#4283=ORIENTED_EDGE('',*,*,#3172,.T.);
#4284=ORIENTED_EDGE('',*,*,#3287,.F.);
#4285=ORIENTED_EDGE('',*,*,#3288,.F.);
#4286=ORIENTED_EDGE('',*,*,#3289,.T.);
#4287=ORIENTED_EDGE('',*,*,#3223,.T.);
#4288=ORIENTED_EDGE('',*,*,#3290,.T.);
#4289=ORIENTED_EDGE('',*,*,#3288,.T.);
#4290=ORIENTED_EDGE('',*,*,#3291,.F.);
#4291=ORIENTED_EDGE('',*,*,#3200,.T.);
#4292=ORIENTED_EDGE('',*,*,#3292,.F.);
#4293=ORIENTED_EDGE('',*,*,#3293,.F.);
#4294=ORIENTED_EDGE('',*,*,#3294,.T.);
#4295=ORIENTED_EDGE('',*,*,#3251,.T.);
#4296=ORIENTED_EDGE('',*,*,#3295,.T.);
#4297=ORIENTED_EDGE('',*,*,#3293,.T.);
#4298=ORIENTED_EDGE('',*,*,#3296,.F.);
#4299=ORIENTED_EDGE('',*,*,#3228,.T.);
#4300=ORIENTED_EDGE('',*,*,#3297,.F.);
#4301=ORIENTED_EDGE('',*,*,#3298,.F.);
#4302=ORIENTED_EDGE('',*,*,#3299,.T.);
#4303=ORIENTED_EDGE('',*,*,#3279,.T.);
#4304=ORIENTED_EDGE('',*,*,#3300,.T.);
#4305=ORIENTED_EDGE('',*,*,#3298,.T.);
#4306=ORIENTED_EDGE('',*,*,#3301,.F.);
#4307=ORIENTED_EDGE('',*,*,#3256,.T.);
#4308=ORIENTED_EDGE('',*,*,#3302,.F.);
#4309=ORIENTED_EDGE('',*,*,#3285,.F.);
#4310=ORIENTED_EDGE('',*,*,#3303,.T.);
#4311=ORIENTED_EDGE('',*,*,#3171,.T.);
#4312=ORIENTED_EDGE('',*,*,#3175,.T.);
#4313=ORIENTED_EDGE('',*,*,#3178,.T.);
#4314=ORIENTED_EDGE('',*,*,#3181,.T.);
#4315=ORIENTED_EDGE('',*,*,#3184,.T.);
#4316=ORIENTED_EDGE('',*,*,#3187,.T.);
#4317=ORIENTED_EDGE('',*,*,#3190,.T.);
#4318=ORIENTED_EDGE('',*,*,#3193,.T.);
#4319=ORIENTED_EDGE('',*,*,#3196,.T.);
#4320=ORIENTED_EDGE('',*,*,#3286,.T.);
#4321=ORIENTED_EDGE('',*,*,#3302,.T.);
#4322=ORIENTED_EDGE('',*,*,#3255,.T.);
#4323=ORIENTED_EDGE('',*,*,#3259,.T.);
#4324=ORIENTED_EDGE('',*,*,#3262,.T.);
#4325=ORIENTED_EDGE('',*,*,#3265,.T.);
#4326=ORIENTED_EDGE('',*,*,#3268,.T.);
#4327=ORIENTED_EDGE('',*,*,#3271,.T.);
#4328=ORIENTED_EDGE('',*,*,#3274,.T.);
#4329=ORIENTED_EDGE('',*,*,#3277,.T.);
#4330=ORIENTED_EDGE('',*,*,#3280,.T.);
#4331=ORIENTED_EDGE('',*,*,#3301,.T.);
#4332=ORIENTED_EDGE('',*,*,#3297,.T.);
#4333=ORIENTED_EDGE('',*,*,#3227,.T.);
#4334=ORIENTED_EDGE('',*,*,#3231,.T.);
#4335=ORIENTED_EDGE('',*,*,#3234,.T.);
#4336=ORIENTED_EDGE('',*,*,#3237,.T.);
#4337=ORIENTED_EDGE('',*,*,#3240,.T.);
#4338=ORIENTED_EDGE('',*,*,#3243,.T.);
#4339=ORIENTED_EDGE('',*,*,#3246,.T.);
#4340=ORIENTED_EDGE('',*,*,#3249,.T.);
#4341=ORIENTED_EDGE('',*,*,#3252,.T.);
#4342=ORIENTED_EDGE('',*,*,#3296,.T.);
#4343=ORIENTED_EDGE('',*,*,#3292,.T.);
#4344=ORIENTED_EDGE('',*,*,#3199,.T.);
#4345=ORIENTED_EDGE('',*,*,#3203,.T.);
#4346=ORIENTED_EDGE('',*,*,#3206,.T.);
#4347=ORIENTED_EDGE('',*,*,#3209,.T.);
#4348=ORIENTED_EDGE('',*,*,#3212,.T.);
#4349=ORIENTED_EDGE('',*,*,#3215,.T.);
#4350=ORIENTED_EDGE('',*,*,#3218,.T.);
#4351=ORIENTED_EDGE('',*,*,#3221,.T.);
#4352=ORIENTED_EDGE('',*,*,#3224,.T.);
#4353=ORIENTED_EDGE('',*,*,#3291,.T.);
#4354=ORIENTED_EDGE('',*,*,#3287,.T.);
#4355=ORIENTED_EDGE('',*,*,#3283,.T.);
#4356=ORIENTED_EDGE('',*,*,#3169,.T.);
#4357=ORIENTED_EDGE('',*,*,#3289,.F.);
#4358=ORIENTED_EDGE('',*,*,#3290,.F.);
#4359=ORIENTED_EDGE('',*,*,#3222,.T.);
#4360=ORIENTED_EDGE('',*,*,#3219,.T.);
#4361=ORIENTED_EDGE('',*,*,#3216,.T.);
#4362=ORIENTED_EDGE('',*,*,#3213,.T.);
#4363=ORIENTED_EDGE('',*,*,#3210,.T.);
#4364=ORIENTED_EDGE('',*,*,#3207,.T.);
#4365=ORIENTED_EDGE('',*,*,#3204,.T.);
#4366=ORIENTED_EDGE('',*,*,#3201,.T.);
#4367=ORIENTED_EDGE('',*,*,#3197,.T.);
#4368=ORIENTED_EDGE('',*,*,#3294,.F.);
#4369=ORIENTED_EDGE('',*,*,#3295,.F.);
#4370=ORIENTED_EDGE('',*,*,#3250,.T.);
#4371=ORIENTED_EDGE('',*,*,#3247,.T.);
#4372=ORIENTED_EDGE('',*,*,#3244,.T.);
#4373=ORIENTED_EDGE('',*,*,#3241,.T.);
#4374=ORIENTED_EDGE('',*,*,#3238,.T.);
#4375=ORIENTED_EDGE('',*,*,#3235,.T.);
#4376=ORIENTED_EDGE('',*,*,#3232,.T.);
#4377=ORIENTED_EDGE('',*,*,#3229,.T.);
#4378=ORIENTED_EDGE('',*,*,#3225,.T.);
#4379=ORIENTED_EDGE('',*,*,#3299,.F.);
#4380=ORIENTED_EDGE('',*,*,#3300,.F.);
#4381=ORIENTED_EDGE('',*,*,#3278,.T.);
#4382=ORIENTED_EDGE('',*,*,#3275,.T.);
#4383=ORIENTED_EDGE('',*,*,#3272,.T.);
#4384=ORIENTED_EDGE('',*,*,#3269,.T.);
#4385=ORIENTED_EDGE('',*,*,#3266,.T.);
#4386=ORIENTED_EDGE('',*,*,#3263,.T.);
#4387=ORIENTED_EDGE('',*,*,#3260,.T.);
#4388=ORIENTED_EDGE('',*,*,#3257,.T.);
#4389=ORIENTED_EDGE('',*,*,#3253,.T.);
#4390=ORIENTED_EDGE('',*,*,#3303,.F.);
#4391=ORIENTED_EDGE('',*,*,#3284,.F.);
#4392=ORIENTED_EDGE('',*,*,#3194,.T.);
#4393=ORIENTED_EDGE('',*,*,#3191,.T.);
#4394=ORIENTED_EDGE('',*,*,#3188,.T.);
#4395=ORIENTED_EDGE('',*,*,#3185,.T.);
#4396=ORIENTED_EDGE('',*,*,#3182,.T.);
#4397=ORIENTED_EDGE('',*,*,#3179,.T.);
#4398=ORIENTED_EDGE('',*,*,#3176,.T.);
#4399=ORIENTED_EDGE('',*,*,#3173,.T.);
#4400=ORIENTED_EDGE('',*,*,#3281,.T.);
#4401=ORIENTED_EDGE('',*,*,#3304,.T.);
#4402=ORIENTED_EDGE('',*,*,#3305,.T.);
#4403=ORIENTED_EDGE('',*,*,#3306,.T.);
#4404=ORIENTED_EDGE('',*,*,#3307,.T.);
#4405=ORIENTED_EDGE('',*,*,#3308,.T.);
#4406=ORIENTED_EDGE('',*,*,#3309,.T.);
#4407=ORIENTED_EDGE('',*,*,#3308,.F.);
#4408=ORIENTED_EDGE('',*,*,#3310,.F.);
#4409=ORIENTED_EDGE('',*,*,#3311,.T.);
#4410=ORIENTED_EDGE('',*,*,#3312,.F.);
#4411=ORIENTED_EDGE('',*,*,#3311,.F.);
#4412=ORIENTED_EDGE('',*,*,#3313,.F.);
#4413=ORIENTED_EDGE('',*,*,#3314,.F.);
#4414=ORIENTED_EDGE('',*,*,#3315,.F.);
#4415=ORIENTED_EDGE('',*,*,#3307,.F.);
#4416=ORIENTED_EDGE('',*,*,#3316,.F.);
#4417=ORIENTED_EDGE('',*,*,#3317,.F.);
#4418=ORIENTED_EDGE('',*,*,#3313,.T.);
#4419=ORIENTED_EDGE('',*,*,#3310,.T.);
#4420=ORIENTED_EDGE('',*,*,#3309,.F.);
#4421=ORIENTED_EDGE('',*,*,#3315,.T.);
#4422=ORIENTED_EDGE('',*,*,#3318,.F.);
#4423=ORIENTED_EDGE('',*,*,#3319,.F.);
#4424=ORIENTED_EDGE('',*,*,#3320,.T.);
#4425=ORIENTED_EDGE('',*,*,#3321,.T.);
#4426=ORIENTED_EDGE('',*,*,#3322,.T.);
#4427=ORIENTED_EDGE('',*,*,#3318,.T.);
#4428=ORIENTED_EDGE('',*,*,#3314,.T.);
#4429=ORIENTED_EDGE('',*,*,#3317,.T.);
#4430=ORIENTED_EDGE('',*,*,#3304,.F.);
#4431=ORIENTED_EDGE('',*,*,#3319,.T.);
#4432=ORIENTED_EDGE('',*,*,#3322,.F.);
#4433=ORIENTED_EDGE('',*,*,#3323,.T.);
#4434=ORIENTED_EDGE('',*,*,#3324,.F.);
#4435=ORIENTED_EDGE('',*,*,#3325,.F.);
#4436=ORIENTED_EDGE('',*,*,#3321,.F.);
#4437=ORIENTED_EDGE('',*,*,#3326,.T.);
#4438=ORIENTED_EDGE('',*,*,#3327,.F.);
#4439=ORIENTED_EDGE('',*,*,#3323,.F.);
#4440=ORIENTED_EDGE('',*,*,#3305,.F.);
#4441=ORIENTED_EDGE('',*,*,#3325,.T.);
#4442=ORIENTED_EDGE('',*,*,#3328,.F.);
#4443=ORIENTED_EDGE('',*,*,#3329,.F.);
#4444=ORIENTED_EDGE('',*,*,#3306,.F.);
#4445=ORIENTED_EDGE('',*,*,#3329,.T.);
#4446=ORIENTED_EDGE('',*,*,#3330,.F.);
#4447=ORIENTED_EDGE('',*,*,#3326,.F.);
#4448=ORIENTED_EDGE('',*,*,#3320,.F.);
#4449=ORIENTED_EDGE('',*,*,#3316,.T.);
#4450=ORIENTED_EDGE('',*,*,#3330,.T.);
#4451=ORIENTED_EDGE('',*,*,#3328,.T.);
#4452=ORIENTED_EDGE('',*,*,#3324,.T.);
#4453=ORIENTED_EDGE('',*,*,#3327,.T.);
#4454=ORIENTED_EDGE('',*,*,#3312,.T.);
#4455=ORIENTED_EDGE('',*,*,#3331,.T.);
#4456=ORIENTED_EDGE('',*,*,#3332,.T.);
#4457=ORIENTED_EDGE('',*,*,#3333,.T.);
#4458=ORIENTED_EDGE('',*,*,#3332,.F.);
#4459=ORIENTED_EDGE('',*,*,#3333,.F.);
#4460=ORIENTED_EDGE('',*,*,#3334,.T.);
#4461=ORIENTED_EDGE('',*,*,#3335,.T.);
#4462=ORIENTED_EDGE('',*,*,#3334,.F.);
#4463=ORIENTED_EDGE('',*,*,#3336,.T.);
#4464=ORIENTED_EDGE('',*,*,#3331,.F.);
#4465=ORIENTED_EDGE('',*,*,#3336,.F.);
#4466=ORIENTED_EDGE('',*,*,#3337,.T.);
#4467=ORIENTED_EDGE('',*,*,#3338,.T.);
#4468=ORIENTED_EDGE('',*,*,#3337,.F.);
#4469=ORIENTED_EDGE('',*,*,#3338,.F.);
#4470=ORIENTED_EDGE('',*,*,#3335,.F.);
#4471=ORIENTED_EDGE('',*,*,#3339,.T.);
#4472=ORIENTED_EDGE('',*,*,#3340,.T.);
#4473=ORIENTED_EDGE('',*,*,#3341,.T.);
#4474=ORIENTED_EDGE('',*,*,#3342,.F.);
#4475=ORIENTED_EDGE('',*,*,#3343,.T.);
#4476=ORIENTED_EDGE('',*,*,#3344,.T.);
#4477=ORIENTED_EDGE('',*,*,#3345,.T.);
#4478=ORIENTED_EDGE('',*,*,#3340,.F.);
#4479=ORIENTED_EDGE('',*,*,#3346,.T.);
#4480=ORIENTED_EDGE('',*,*,#3347,.T.);
#4481=ORIENTED_EDGE('',*,*,#3348,.T.);
#4482=ORIENTED_EDGE('',*,*,#3344,.F.);
#4483=ORIENTED_EDGE('',*,*,#3349,.T.);
#4484=ORIENTED_EDGE('',*,*,#3350,.T.);
#4485=ORIENTED_EDGE('',*,*,#3351,.T.);
#4486=ORIENTED_EDGE('',*,*,#3347,.F.);
#4487=ORIENTED_EDGE('',*,*,#3352,.T.);
#4488=ORIENTED_EDGE('',*,*,#3353,.T.);
#4489=ORIENTED_EDGE('',*,*,#3354,.T.);
#4490=ORIENTED_EDGE('',*,*,#3350,.F.);
#4491=ORIENTED_EDGE('',*,*,#3355,.T.);
#4492=ORIENTED_EDGE('',*,*,#3342,.T.);
#4493=ORIENTED_EDGE('',*,*,#3356,.T.);
#4494=ORIENTED_EDGE('',*,*,#3353,.F.);
#4495=ORIENTED_EDGE('',*,*,#3355,.F.);
#4496=ORIENTED_EDGE('',*,*,#3352,.F.);
#4497=ORIENTED_EDGE('',*,*,#3349,.F.);
#4498=ORIENTED_EDGE('',*,*,#3346,.F.);
#4499=ORIENTED_EDGE('',*,*,#3343,.F.);
#4500=ORIENTED_EDGE('',*,*,#3339,.F.);
#4501=ORIENTED_EDGE('',*,*,#3356,.F.);
#4502=ORIENTED_EDGE('',*,*,#3341,.F.);
#4503=ORIENTED_EDGE('',*,*,#3345,.F.);
#4504=ORIENTED_EDGE('',*,*,#3348,.F.);
#4505=ORIENTED_EDGE('',*,*,#3351,.F.);
#4506=ORIENTED_EDGE('',*,*,#3354,.F.);
#4507=ORIENTED_EDGE('',*,*,#3357,.F.);
#4508=ORIENTED_EDGE('',*,*,#3358,.F.);
#4509=ORIENTED_EDGE('',*,*,#3359,.F.);
#4510=ORIENTED_EDGE('',*,*,#3360,.T.);
#4511=ORIENTED_EDGE('',*,*,#3358,.T.);
#4512=ORIENTED_EDGE('',*,*,#3360,.F.);
#4513=ORIENTED_EDGE('',*,*,#3361,.F.);
#4514=ORIENTED_EDGE('',*,*,#3362,.T.);
#4515=ORIENTED_EDGE('',*,*,#3359,.T.);
#4516=ORIENTED_EDGE('',*,*,#3362,.F.);
#4517=ORIENTED_EDGE('',*,*,#3363,.F.);
#4518=ORIENTED_EDGE('',*,*,#3364,.T.);
#4519=ORIENTED_EDGE('',*,*,#3361,.T.);
#4520=ORIENTED_EDGE('',*,*,#3364,.F.);
#4521=ORIENTED_EDGE('',*,*,#3363,.T.);
#4522=ORIENTED_EDGE('',*,*,#3365,.F.);
#4523=ORIENTED_EDGE('',*,*,#3366,.F.);
#4524=ORIENTED_EDGE('',*,*,#3367,.T.);
#4525=ORIENTED_EDGE('',*,*,#3365,.T.);
#4526=ORIENTED_EDGE('',*,*,#3367,.F.);
#4527=ORIENTED_EDGE('',*,*,#3357,.T.);
#4528=ORIENTED_EDGE('',*,*,#3368,.T.);
#4529=ORIENTED_EDGE('',*,*,#3366,.T.);
#4530=ORIENTED_EDGE('',*,*,#3368,.F.);
#4531=ORIENTED_EDGE('',*,*,#3369,.F.);
#4532=ORIENTED_EDGE('',*,*,#3370,.T.);
#4533=ORIENTED_EDGE('',*,*,#3371,.F.);
#4534=ORIENTED_EDGE('',*,*,#3370,.F.);
#4535=ORIENTED_EDGE('',*,*,#3372,.F.);
#4536=ORIENTED_EDGE('',*,*,#3373,.T.);
#4537=ORIENTED_EDGE('',*,*,#3369,.T.);
#4538=ORIENTED_EDGE('',*,*,#3373,.F.);
#4539=ORIENTED_EDGE('',*,*,#3372,.T.);
#4540=ORIENTED_EDGE('',*,*,#3374,.F.);
#4541=ORIENTED_EDGE('',*,*,#3375,.T.);
#4542=ORIENTED_EDGE('',*,*,#3376,.F.);
#4543=ORIENTED_EDGE('',*,*,#3377,.F.);
#4544=ORIENTED_EDGE('',*,*,#3378,.F.);
#4545=ORIENTED_EDGE('',*,*,#3379,.F.);
#4546=ORIENTED_EDGE('',*,*,#3380,.F.);
#4547=ORIENTED_EDGE('',*,*,#3381,.F.);
#4548=ORIENTED_EDGE('',*,*,#3375,.F.);
#4549=ORIENTED_EDGE('',*,*,#3380,.T.);
#4550=ORIENTED_EDGE('',*,*,#3382,.F.);
#4551=ORIENTED_EDGE('',*,*,#3383,.T.);
#4552=ORIENTED_EDGE('',*,*,#3384,.T.);
#4553=ORIENTED_EDGE('',*,*,#3379,.T.);
#4554=ORIENTED_EDGE('',*,*,#3385,.F.);
#4555=ORIENTED_EDGE('',*,*,#3386,.T.);
#4556=ORIENTED_EDGE('',*,*,#3382,.T.);
#4557=ORIENTED_EDGE('',*,*,#3378,.T.);
#4558=ORIENTED_EDGE('',*,*,#3387,.F.);
#4559=ORIENTED_EDGE('',*,*,#3388,.T.);
#4560=ORIENTED_EDGE('',*,*,#3385,.T.);
#4561=ORIENTED_EDGE('',*,*,#3377,.T.);
#4562=ORIENTED_EDGE('',*,*,#3389,.F.);
#4563=ORIENTED_EDGE('',*,*,#3390,.T.);
#4564=ORIENTED_EDGE('',*,*,#3387,.T.);
#4565=ORIENTED_EDGE('',*,*,#3376,.T.);
#4566=ORIENTED_EDGE('',*,*,#3391,.F.);
#4567=ORIENTED_EDGE('',*,*,#3392,.T.);
#4568=ORIENTED_EDGE('',*,*,#3389,.T.);
#4569=ORIENTED_EDGE('',*,*,#3381,.T.);
#4570=ORIENTED_EDGE('',*,*,#3384,.F.);
#4571=ORIENTED_EDGE('',*,*,#3393,.T.);
#4572=ORIENTED_EDGE('',*,*,#3391,.T.);
#4573=ORIENTED_EDGE('',*,*,#3374,.T.);
#4574=ORIENTED_EDGE('',*,*,#3388,.F.);
#4575=ORIENTED_EDGE('',*,*,#3390,.F.);
#4576=ORIENTED_EDGE('',*,*,#3392,.F.);
#4577=ORIENTED_EDGE('',*,*,#3393,.F.);
#4578=ORIENTED_EDGE('',*,*,#3383,.F.);
#4579=ORIENTED_EDGE('',*,*,#3386,.F.);
#4580=ORIENTED_EDGE('',*,*,#3371,.T.);
#4581=ORIENTED_EDGE('',*,*,#3394,.F.);
#4582=ORIENTED_EDGE('',*,*,#3395,.F.);
#4583=ORIENTED_EDGE('',*,*,#3396,.T.);
#4584=ORIENTED_EDGE('',*,*,#3397,.F.);
#4585=ORIENTED_EDGE('',*,*,#3396,.F.);
#4586=ORIENTED_EDGE('',*,*,#3398,.F.);
#4587=ORIENTED_EDGE('',*,*,#3399,.F.);
#4588=ORIENTED_EDGE('',*,*,#3400,.F.);
#4589=ORIENTED_EDGE('',*,*,#3401,.F.);
#4590=ORIENTED_EDGE('',*,*,#3402,.F.);
#4591=ORIENTED_EDGE('',*,*,#3403,.T.);
#4592=ORIENTED_EDGE('',*,*,#3404,.F.);
#4593=ORIENTED_EDGE('',*,*,#3405,.F.);
#4594=ORIENTED_EDGE('',*,*,#3406,.F.);
#4595=ORIENTED_EDGE('',*,*,#3407,.F.);
#4596=ORIENTED_EDGE('',*,*,#3408,.F.);
#4597=ORIENTED_EDGE('',*,*,#3409,.F.);
#4598=ORIENTED_EDGE('',*,*,#3403,.F.);
#4599=ORIENTED_EDGE('',*,*,#3399,.T.);
#4600=ORIENTED_EDGE('',*,*,#3410,.T.);
#4601=ORIENTED_EDGE('',*,*,#3408,.T.);
#4602=ORIENTED_EDGE('',*,*,#3411,.F.);
#4603=ORIENTED_EDGE('',*,*,#3398,.T.);
#4604=ORIENTED_EDGE('',*,*,#3412,.T.);
#4605=ORIENTED_EDGE('',*,*,#3409,.T.);
#4606=ORIENTED_EDGE('',*,*,#3410,.F.);
#4607=ORIENTED_EDGE('',*,*,#3395,.T.);
#4608=ORIENTED_EDGE('',*,*,#3413,.T.);
#4609=ORIENTED_EDGE('',*,*,#3404,.T.);
#4610=ORIENTED_EDGE('',*,*,#3412,.F.);
#4611=ORIENTED_EDGE('',*,*,#3414,.F.);
#4612=ORIENTED_EDGE('',*,*,#3415,.T.);
#4613=ORIENTED_EDGE('',*,*,#3416,.T.);
#4614=ORIENTED_EDGE('',*,*,#3415,.F.);
#4615=ORIENTED_EDGE('',*,*,#3394,.T.);
#4616=ORIENTED_EDGE('',*,*,#3417,.T.);
#4617=ORIENTED_EDGE('',*,*,#3405,.T.);
#4618=ORIENTED_EDGE('',*,*,#3413,.F.);
#4619=ORIENTED_EDGE('',*,*,#3400,.T.);
#4620=ORIENTED_EDGE('',*,*,#3411,.T.);
#4621=ORIENTED_EDGE('',*,*,#3407,.T.);
#4622=ORIENTED_EDGE('',*,*,#3418,.F.);
#4623=ORIENTED_EDGE('',*,*,#3401,.T.);
#4624=ORIENTED_EDGE('',*,*,#3418,.T.);
#4625=ORIENTED_EDGE('',*,*,#3406,.T.);
#4626=ORIENTED_EDGE('',*,*,#3417,.F.);
#4627=ORIENTED_EDGE('',*,*,#3402,.T.);
#4628=ORIENTED_EDGE('',*,*,#3414,.T.);
#4629=ORIENTED_EDGE('',*,*,#3397,.T.);
#4630=ORIENTED_EDGE('',*,*,#3416,.F.);
#4631=ORIENTED_EDGE('',*,*,#3419,.F.);
#4632=ORIENTED_EDGE('',*,*,#3420,.T.);
#4633=ORIENTED_EDGE('',*,*,#3421,.F.);
#4634=ORIENTED_EDGE('',*,*,#3420,.F.);
#4635=ORIENTED_EDGE('',*,*,#3422,.F.);
#4636=ORIENTED_EDGE('',*,*,#3423,.T.);
#4637=ORIENTED_EDGE('',*,*,#3424,.F.);
#4638=ORIENTED_EDGE('',*,*,#3423,.F.);
#4639=ORIENTED_EDGE('',*,*,#3425,.F.);
#4640=ORIENTED_EDGE('',*,*,#3426,.T.);
#4641=ORIENTED_EDGE('',*,*,#3427,.F.);
#4642=ORIENTED_EDGE('',*,*,#3426,.F.);
#4643=ORIENTED_EDGE('',*,*,#3428,.F.);
#4644=ORIENTED_EDGE('',*,*,#3429,.T.);
#4645=ORIENTED_EDGE('',*,*,#3430,.F.);
#4646=ORIENTED_EDGE('',*,*,#3429,.F.);
#4647=ORIENTED_EDGE('',*,*,#3431,.F.);
#4648=ORIENTED_EDGE('',*,*,#3432,.T.);
#4649=ORIENTED_EDGE('',*,*,#3433,.T.);
#4650=ORIENTED_EDGE('',*,*,#3432,.F.);
#4651=ORIENTED_EDGE('',*,*,#3434,.F.);
#4652=ORIENTED_EDGE('',*,*,#3433,.F.);
#4653=ORIENTED_EDGE('',*,*,#3434,.T.);
#4654=ORIENTED_EDGE('',*,*,#3435,.T.);
#4655=ORIENTED_EDGE('',*,*,#3436,.T.);
#4656=ORIENTED_EDGE('',*,*,#3435,.F.);
#4657=ORIENTED_EDGE('',*,*,#3437,.F.);
#4658=ORIENTED_EDGE('',*,*,#3438,.T.);
#4659=ORIENTED_EDGE('',*,*,#3439,.T.);
#4660=ORIENTED_EDGE('',*,*,#3438,.F.);
#4661=ORIENTED_EDGE('',*,*,#3437,.T.);
#4662=ORIENTED_EDGE('',*,*,#3431,.T.);
#4663=ORIENTED_EDGE('',*,*,#3430,.T.);
#4664=ORIENTED_EDGE('',*,*,#3427,.T.);
#4665=ORIENTED_EDGE('',*,*,#3424,.T.);
#4666=ORIENTED_EDGE('',*,*,#3421,.T.);
#4667=ORIENTED_EDGE('',*,*,#3439,.F.);
#4668=ORIENTED_EDGE('',*,*,#3436,.F.);
#4669=ORIENTED_EDGE('',*,*,#3428,.T.);
#4670=ORIENTED_EDGE('',*,*,#3425,.T.);
#4671=ORIENTED_EDGE('',*,*,#3422,.T.);
#4672=ORIENTED_EDGE('',*,*,#3419,.T.);
#4673=ORIENTED_EDGE('',*,*,#3440,.F.);
#4674=ORIENTED_EDGE('',*,*,#3441,.T.);
#4675=ORIENTED_EDGE('',*,*,#3442,.F.);
#4676=ORIENTED_EDGE('',*,*,#3441,.F.);
#4677=ORIENTED_EDGE('',*,*,#3443,.F.);
#4678=ORIENTED_EDGE('',*,*,#3444,.T.);
#4679=ORIENTED_EDGE('',*,*,#3445,.F.);
#4680=ORIENTED_EDGE('',*,*,#3444,.F.);
#4681=ORIENTED_EDGE('',*,*,#3446,.F.);
#4682=ORIENTED_EDGE('',*,*,#3447,.T.);
#4683=ORIENTED_EDGE('',*,*,#3448,.F.);
#4684=ORIENTED_EDGE('',*,*,#3447,.F.);
#4685=ORIENTED_EDGE('',*,*,#3449,.F.);
#4686=ORIENTED_EDGE('',*,*,#3450,.T.);
#4687=ORIENTED_EDGE('',*,*,#3451,.F.);
#4688=ORIENTED_EDGE('',*,*,#3450,.F.);
#4689=ORIENTED_EDGE('',*,*,#3452,.F.);
#4690=ORIENTED_EDGE('',*,*,#3453,.T.);
#4691=ORIENTED_EDGE('',*,*,#3454,.T.);
#4692=ORIENTED_EDGE('',*,*,#3453,.F.);
#4693=ORIENTED_EDGE('',*,*,#3455,.F.);
#4694=ORIENTED_EDGE('',*,*,#3452,.T.);
#4695=ORIENTED_EDGE('',*,*,#3456,.F.);
#4696=ORIENTED_EDGE('',*,*,#3457,.T.);
#4697=ORIENTED_EDGE('',*,*,#3455,.T.);
#4698=ORIENTED_EDGE('',*,*,#3457,.F.);
#4699=ORIENTED_EDGE('',*,*,#3458,.F.);
#4700=ORIENTED_EDGE('',*,*,#3459,.T.);
#4701=ORIENTED_EDGE('',*,*,#3460,.T.);
#4702=ORIENTED_EDGE('',*,*,#3459,.F.);
#4703=ORIENTED_EDGE('',*,*,#3458,.T.);
#4704=ORIENTED_EDGE('',*,*,#3456,.T.);
#4705=ORIENTED_EDGE('',*,*,#3451,.T.);
#4706=ORIENTED_EDGE('',*,*,#3448,.T.);
#4707=ORIENTED_EDGE('',*,*,#3445,.T.);
#4708=ORIENTED_EDGE('',*,*,#3442,.T.);
#4709=ORIENTED_EDGE('',*,*,#3460,.F.);
#4710=ORIENTED_EDGE('',*,*,#3454,.F.);
#4711=ORIENTED_EDGE('',*,*,#3449,.T.);
#4712=ORIENTED_EDGE('',*,*,#3446,.T.);
#4713=ORIENTED_EDGE('',*,*,#3443,.T.);
#4714=ORIENTED_EDGE('',*,*,#3440,.T.);
#4715=ORIENTED_EDGE('',*,*,#3461,.F.);
#4716=ORIENTED_EDGE('',*,*,#3462,.T.);
#4717=ORIENTED_EDGE('',*,*,#3463,.T.);
#4718=ORIENTED_EDGE('',*,*,#3462,.F.);
#4719=ORIENTED_EDGE('',*,*,#3464,.F.);
#4720=ORIENTED_EDGE('',*,*,#3465,.T.);
#4721=ORIENTED_EDGE('',*,*,#3466,.T.);
#4722=ORIENTED_EDGE('',*,*,#3465,.F.);
#4723=ORIENTED_EDGE('',*,*,#3464,.T.);
#4724=ORIENTED_EDGE('',*,*,#3461,.T.);
#4725=ORIENTED_EDGE('',*,*,#3466,.F.);
#4726=ORIENTED_EDGE('',*,*,#3463,.F.);
#4727=ORIENTED_EDGE('',*,*,#3467,.F.);
#4728=ORIENTED_EDGE('',*,*,#3468,.T.);
#4729=ORIENTED_EDGE('',*,*,#3469,.F.);
#4730=ORIENTED_EDGE('',*,*,#3468,.F.);
#4731=ORIENTED_EDGE('',*,*,#3470,.F.);
#4732=ORIENTED_EDGE('',*,*,#3471,.T.);
#4733=ORIENTED_EDGE('',*,*,#3472,.F.);
#4734=ORIENTED_EDGE('',*,*,#3471,.F.);
#4735=ORIENTED_EDGE('',*,*,#3473,.F.);
#4736=ORIENTED_EDGE('',*,*,#3474,.T.);
#4737=ORIENTED_EDGE('',*,*,#3475,.F.);
#4738=ORIENTED_EDGE('',*,*,#3474,.F.);
#4739=ORIENTED_EDGE('',*,*,#3476,.F.);
#4740=ORIENTED_EDGE('',*,*,#3477,.T.);
#4741=ORIENTED_EDGE('',*,*,#3478,.F.);
#4742=ORIENTED_EDGE('',*,*,#3477,.F.);
#4743=ORIENTED_EDGE('',*,*,#3479,.F.);
#4744=ORIENTED_EDGE('',*,*,#3480,.T.);
#4745=ORIENTED_EDGE('',*,*,#3481,.T.);
#4746=ORIENTED_EDGE('',*,*,#3480,.F.);
#4747=ORIENTED_EDGE('',*,*,#3482,.F.);
#4748=ORIENTED_EDGE('',*,*,#3483,.T.);
#4749=ORIENTED_EDGE('',*,*,#3484,.T.);
#4750=ORIENTED_EDGE('',*,*,#3483,.F.);
#4751=ORIENTED_EDGE('',*,*,#3482,.T.);
#4752=ORIENTED_EDGE('',*,*,#3479,.T.);
#4753=ORIENTED_EDGE('',*,*,#3478,.T.);
#4754=ORIENTED_EDGE('',*,*,#3475,.T.);
#4755=ORIENTED_EDGE('',*,*,#3472,.T.);
#4756=ORIENTED_EDGE('',*,*,#3469,.T.);
#4757=ORIENTED_EDGE('',*,*,#3484,.F.);
#4758=ORIENTED_EDGE('',*,*,#3481,.F.);
#4759=ORIENTED_EDGE('',*,*,#3476,.T.);
#4760=ORIENTED_EDGE('',*,*,#3473,.T.);
#4761=ORIENTED_EDGE('',*,*,#3470,.T.);
#4762=ORIENTED_EDGE('',*,*,#3467,.T.);
#4763=ORIENTED_EDGE('',*,*,#3485,.F.);
#4764=ORIENTED_EDGE('',*,*,#3486,.F.);
#4765=ORIENTED_EDGE('',*,*,#3487,.T.);
#4766=ORIENTED_EDGE('',*,*,#3485,.T.);
#4767=ORIENTED_EDGE('',*,*,#3487,.F.);
#4768=ORIENTED_EDGE('',*,*,#3488,.F.);
#4769=ORIENTED_EDGE('',*,*,#3489,.T.);
#4770=ORIENTED_EDGE('',*,*,#3486,.T.);
#4771=ORIENTED_EDGE('',*,*,#3489,.F.);
#4772=ORIENTED_EDGE('',*,*,#3490,.F.);
#4773=ORIENTED_EDGE('',*,*,#3491,.T.);
#4774=ORIENTED_EDGE('',*,*,#3488,.T.);
#4775=ORIENTED_EDGE('',*,*,#3491,.F.);
#4776=ORIENTED_EDGE('',*,*,#3490,.T.);
#4777=ORIENTED_EDGE('',*,*,#3492,.F.);
#4778=ORIENTED_EDGE('',*,*,#3493,.F.);
#4779=ORIENTED_EDGE('',*,*,#3494,.T.);
#4780=ORIENTED_EDGE('',*,*,#3492,.T.);
#4781=ORIENTED_EDGE('',*,*,#3494,.F.);
#4782=ORIENTED_EDGE('',*,*,#3495,.F.);
#4783=ORIENTED_EDGE('',*,*,#3496,.T.);
#4784=ORIENTED_EDGE('',*,*,#3493,.T.);
#4785=ORIENTED_EDGE('',*,*,#3496,.F.);
#4786=ORIENTED_EDGE('',*,*,#3497,.F.);
#4787=ORIENTED_EDGE('',*,*,#3498,.T.);
#4788=ORIENTED_EDGE('',*,*,#3495,.T.);
#4789=ORIENTED_EDGE('',*,*,#3498,.F.);
#4790=ORIENTED_EDGE('',*,*,#3497,.T.);
#4791=ORIENTED_EDGE('',*,*,#3499,.T.);
#4792=ORIENTED_EDGE('',*,*,#3500,.T.);
#4793=ORIENTED_EDGE('',*,*,#3501,.T.);
#4794=ORIENTED_EDGE('',*,*,#3502,.F.);
#4795=ORIENTED_EDGE('',*,*,#3503,.T.);
#4796=ORIENTED_EDGE('',*,*,#3504,.T.);
#4797=ORIENTED_EDGE('',*,*,#3505,.T.);
#4798=ORIENTED_EDGE('',*,*,#3500,.F.);
#4799=ORIENTED_EDGE('',*,*,#3506,.T.);
#4800=ORIENTED_EDGE('',*,*,#3507,.T.);
#4801=ORIENTED_EDGE('',*,*,#3508,.T.);
#4802=ORIENTED_EDGE('',*,*,#3504,.F.);
#4803=ORIENTED_EDGE('',*,*,#3509,.T.);
#4804=ORIENTED_EDGE('',*,*,#3510,.T.);
#4805=ORIENTED_EDGE('',*,*,#3511,.T.);
#4806=ORIENTED_EDGE('',*,*,#3507,.F.);
#4807=ORIENTED_EDGE('',*,*,#3512,.T.);
#4808=ORIENTED_EDGE('',*,*,#3513,.T.);
#4809=ORIENTED_EDGE('',*,*,#3514,.T.);
#4810=ORIENTED_EDGE('',*,*,#3510,.F.);
#4811=ORIENTED_EDGE('',*,*,#3515,.T.);
#4812=ORIENTED_EDGE('',*,*,#3502,.T.);
#4813=ORIENTED_EDGE('',*,*,#3516,.T.);
#4814=ORIENTED_EDGE('',*,*,#3513,.F.);
#4815=ORIENTED_EDGE('',*,*,#3515,.F.);
#4816=ORIENTED_EDGE('',*,*,#3512,.F.);
#4817=ORIENTED_EDGE('',*,*,#3509,.F.);
#4818=ORIENTED_EDGE('',*,*,#3506,.F.);
#4819=ORIENTED_EDGE('',*,*,#3503,.F.);
#4820=ORIENTED_EDGE('',*,*,#3499,.F.);
#4821=ORIENTED_EDGE('',*,*,#3516,.F.);
#4822=ORIENTED_EDGE('',*,*,#3501,.F.);
#4823=ORIENTED_EDGE('',*,*,#3505,.F.);
#4824=ORIENTED_EDGE('',*,*,#3508,.F.);
#4825=ORIENTED_EDGE('',*,*,#3511,.F.);
#4826=ORIENTED_EDGE('',*,*,#3514,.F.);
#4827=CYLINDRICAL_SURFACE('',#5512,0.165);
#4828=CYLINDRICAL_SURFACE('',#5516,0.165);
#4829=CYLINDRICAL_SURFACE('',#5526,0.6);
#4830=CYLINDRICAL_SURFACE('',#5527,0.5);
#4831=CYLINDRICAL_SURFACE('',#5529,0.5);
#4832=CYLINDRICAL_SURFACE('',#5534,0.505);
#4833=CYLINDRICAL_SURFACE('',#5537,0.8);
#4834=CYLINDRICAL_SURFACE('',#5543,0.505);
#4835=CYLINDRICAL_SURFACE('',#5546,0.8);
#4836=CYLINDRICAL_SURFACE('',#5552,0.225);
#4837=CYLINDRICAL_SURFACE('',#5555,1.1);
#4838=CYLINDRICAL_SURFACE('',#5561,0.605);
#4839=CYLINDRICAL_SURFACE('',#5564,1.);
#4840=CYLINDRICAL_SURFACE('',#5577,0.976185);
#4841=CYLINDRICAL_SURFACE('',#5579,0.5);
#4842=CYLINDRICAL_SURFACE('',#5585,0.976185);
#4843=CYLINDRICAL_SURFACE('',#5597,1.023815);
#4844=CYLINDRICAL_SURFACE('',#5604,1.5);
#4845=CYLINDRICAL_SURFACE('',#5609,1.023815);
#4846=CYLINDRICAL_SURFACE('',#5631,1.019052);
#4847=CYLINDRICAL_SURFACE('',#5671,0.980948);
#4848=CYLINDRICAL_SURFACE('',#5685,1.013815);
#4849=CYLINDRICAL_SURFACE('',#5689,0.991185);
#4850=CYLINDRICAL_SURFACE('',#5693,1.013815);
#4851=CYLINDRICAL_SURFACE('',#5697,0.991185);
#4852=CYLINDRICAL_SURFACE('',#5704,0.525);
#4853=CYLINDRICAL_SURFACE('',#5707,0.525);
#4854=CYLINDRICAL_SURFACE('',#5719,0.275);
#4855=CYLINDRICAL_SURFACE('',#5722,0.525);
#4856=CYLINDRICAL_SURFACE('',#5725,0.525);
#4857=CYLINDRICAL_SURFACE('',#5730,0.275);
#4858=CYLINDRICAL_SURFACE('',#5733,0.505);
#4859=CYLINDRICAL_SURFACE('',#5743,0.275);
#4860=CYLINDRICAL_SURFACE('',#5746,0.34);
#4861=CYLINDRICAL_SURFACE('',#5758,0.525);
#4862=CYLINDRICAL_SURFACE('',#5761,0.525);
#4863=CYLINDRICAL_SURFACE('',#5773,0.275);
#4864=CYLINDRICAL_SURFACE('',#5776,0.525);
#4865=CYLINDRICAL_SURFACE('',#5779,0.525);
#4866=CYLINDRICAL_SURFACE('',#5784,0.275);
#4867=CYLINDRICAL_SURFACE('',#5787,0.505);
#4868=CYLINDRICAL_SURFACE('',#5797,0.275);
#4869=CYLINDRICAL_SURFACE('',#5800,0.34);
#4870=CYLINDRICAL_SURFACE('',#5848,0.21);
#4871=CYLINDRICAL_SURFACE('',#5864,0.2117);
#4872=CYLINDRICAL_SURFACE('',#5882,0.265);
#4873=CYLINDRICAL_SURFACE('',#5886,0.5);
#4874=CYLINDRICAL_SURFACE('',#5904,0.425);
#4875=CYLINDRICAL_SURFACE('',#5912,0.24505);
#4876=CYLINDRICAL_SURFACE('',#5914,0.3933);
#4877=CYLINDRICAL_SURFACE('',#5938,0.338975);
#4878=CYLINDRICAL_SURFACE('',#5948,0.165);
#4879=CYLINDRICAL_SURFACE('',#5951,0.165);
#4880=CYLINDRICAL_SURFACE('',#5954,0.165);
#4881=CYLINDRICAL_SURFACE('',#5957,0.165);
#4882=CYLINDRICAL_SURFACE('',#5960,1.2);
#4883=CYLINDRICAL_SURFACE('',#5965,1.5);
#4884=CYLINDRICAL_SURFACE('',#5967,2.2);
#4885=CYLINDRICAL_SURFACE('',#5973,0.165);
#4886=CYLINDRICAL_SURFACE('',#5976,0.165);
#4887=CYLINDRICAL_SURFACE('',#5979,0.165);
#4888=CYLINDRICAL_SURFACE('',#5982,0.165);
#4889=CYLINDRICAL_SURFACE('',#5985,1.2);
#4890=CYLINDRICAL_SURFACE('',#5990,1.5);
#4891=CYLINDRICAL_SURFACE('',#5992,2.2);
#4892=CYLINDRICAL_SURFACE('',#5998,2.2);
#4893=CYLINDRICAL_SURFACE('',#6001,2.5);
#4894=CYLINDRICAL_SURFACE('',#6007,0.225);
#4895=CYLINDRICAL_SURFACE('',#6010,0.225);
#4896=CYLINDRICAL_SURFACE('',#6013,0.225);
#4897=CYLINDRICAL_SURFACE('',#6016,0.225);
#4898=CYLINDRICAL_SURFACE('',#6019,1.2);
#4899=CYLINDRICAL_SURFACE('',#6022,2.5);
#4900=CYLINDRICAL_SURFACE('',#6032,0.35);
#4901=CYLINDRICAL_SURFACE('',#6040,0.1954);
#4902=ADVANCED_FACE('',(#715),#4827,.F.);
#4903=ADVANCED_FACE('',(#716),#528,.T.);
#4904=ADVANCED_FACE('',(#717),#4828,.F.);
#4905=ADVANCED_FACE('',(#718),#529,.F.);
#4906=ADVANCED_FACE('',(#719,#437),#530,.T.);
#4907=ADVANCED_FACE('',(#720,#438),#531,.F.);
#4908=ADVANCED_FACE('',(#721),#4829,.T.);
#4909=ADVANCED_FACE('',(#722),#4830,.T.);
#4910=ADVANCED_FACE('',(#723),#4831,.T.);
#4911=ADVANCED_FACE('',(#724,#439),#532,.T.);
#4912=ADVANCED_FACE('',(#725,#440),#533,.F.);
#4913=ADVANCED_FACE('',(#726),#4832,.F.);
#4914=ADVANCED_FACE('',(#727),#4833,.T.);
#4915=ADVANCED_FACE('',(#728,#441),#534,.T.);
#4916=ADVANCED_FACE('',(#729,#442),#535,.F.);
#4917=ADVANCED_FACE('',(#730),#4834,.F.);
#4918=ADVANCED_FACE('',(#731),#4835,.T.);
#4919=ADVANCED_FACE('',(#732,#443),#536,.T.);
#4920=ADVANCED_FACE('',(#733,#444),#537,.F.);
#4921=ADVANCED_FACE('',(#734),#4836,.F.);
#4922=ADVANCED_FACE('',(#735),#4837,.T.);
#4923=ADVANCED_FACE('',(#736,#445),#538,.T.);
#4924=ADVANCED_FACE('',(#737,#446),#539,.F.);
#4925=ADVANCED_FACE('',(#738),#4838,.F.);
#4926=ADVANCED_FACE('',(#739),#4839,.T.);
#4927=ADVANCED_FACE('',(#740,#447),#540,.T.);
#4928=ADVANCED_FACE('',(#741,#448),#541,.F.);
#4929=ADVANCED_FACE('',(#742),#321,.F.);
#4930=ADVANCED_FACE('',(#743),#4840,.T.);
#4931=ADVANCED_FACE('',(#744),#4841,.F.);
#4932=ADVANCED_FACE('',(#745),#305,.F.);
#4933=ADVANCED_FACE('',(#746,#449),#542,.T.);
#4934=ADVANCED_FACE('',(#747),#4842,.T.);
#4935=ADVANCED_FACE('',(#748,#450),#543,.T.);
#4936=ADVANCED_FACE('',(#749),#306,.F.);
#4937=ADVANCED_FACE('',(#750),#322,.F.);
#4938=ADVANCED_FACE('',(#751),#4843,.F.);
#4939=ADVANCED_FACE('',(#752,#451),#544,.T.);
#4940=ADVANCED_FACE('',(#753),#307,.T.);
#4941=ADVANCED_FACE('',(#754),#4844,.T.);
#4942=ADVANCED_FACE('',(#755),#308,.T.);
#4943=ADVANCED_FACE('',(#756,#452),#545,.T.);
#4944=ADVANCED_FACE('',(#757),#4845,.F.);
#4945=ADVANCED_FACE('',(#758),#289,.T.);
#4946=ADVANCED_FACE('',(#759),#290,.T.);
#4947=ADVANCED_FACE('',(#760),#291,.T.);
#4948=ADVANCED_FACE('',(#761),#292,.T.);
#4949=ADVANCED_FACE('',(#762),#293,.T.);
#4950=ADVANCED_FACE('',(#763),#294,.T.);
#4951=ADVANCED_FACE('',(#764),#295,.T.);
#4952=ADVANCED_FACE('',(#765),#296,.T.);
#4953=ADVANCED_FACE('',(#766),#297,.F.);
#4954=ADVANCED_FACE('',(#767),#4846,.T.);
#4955=ADVANCED_FACE('',(#768),#546,.T.);
#4956=ADVANCED_FACE('',(#769),#298,.F.);
#4957=ADVANCED_FACE('',(#770),#547,.T.);
#4958=ADVANCED_FACE('',(#771),#299,.F.);
#4959=ADVANCED_FACE('',(#772),#548,.T.);
#4960=ADVANCED_FACE('',(#773),#300,.F.);
#4961=ADVANCED_FACE('',(#774),#549,.T.);
#4962=ADVANCED_FACE('',(#775),#301,.F.);
#4963=ADVANCED_FACE('',(#776),#550,.T.);
#4964=ADVANCED_FACE('',(#777),#302,.F.);
#4965=ADVANCED_FACE('',(#778),#551,.T.);
#4966=ADVANCED_FACE('',(#779),#303,.F.);
#4967=ADVANCED_FACE('',(#780),#4847,.F.);
#4968=ADVANCED_FACE('',(#781),#552,.T.);
#4969=ADVANCED_FACE('',(#782),#304,.F.);
#4970=ADVANCED_FACE('',(#783,#453),#553,.T.);
#4971=ADVANCED_FACE('',(#784),#554,.T.);
#4972=ADVANCED_FACE('',(#785,#454),#555,.T.);
#4973=ADVANCED_FACE('',(#786),#4848,.T.);
#4974=ADVANCED_FACE('',(#787,#455),#556,.T.);
#4975=ADVANCED_FACE('',(#788),#4849,.F.);
#4976=ADVANCED_FACE('',(#789,#456),#557,.T.);
#4977=ADVANCED_FACE('',(#790),#4850,.T.);
#4978=ADVANCED_FACE('',(#791,#457),#558,.T.);
#4979=ADVANCED_FACE('',(#792),#4851,.F.);
#4980=ADVANCED_FACE('',(#793),#4852,.F.);
#4981=ADVANCED_FACE('',(#794),#4853,.F.);
#4982=ADVANCED_FACE('',(#795),#559,.F.);
#4983=ADVANCED_FACE('',(#796,#458),#560,.F.);
#4984=ADVANCED_FACE('',(#797),#561,.T.);
#4985=ADVANCED_FACE('',(#798),#562,.T.);
#4986=ADVANCED_FACE('',(#799),#563,.T.);
#4987=ADVANCED_FACE('',(#800,#459),#564,.T.);
#4988=ADVANCED_FACE('',(#801),#4854,.F.);
#4989=ADVANCED_FACE('',(#802),#4855,.F.);
#4990=ADVANCED_FACE('',(#803),#4856,.F.);
#4991=ADVANCED_FACE('',(#804),#565,.T.);
#4992=ADVANCED_FACE('',(#805),#566,.T.);
#4993=ADVANCED_FACE('',(#806),#567,.F.);
#4994=ADVANCED_FACE('',(#807),#4857,.F.);
#4995=ADVANCED_FACE('',(#808),#4858,.F.);
#4996=ADVANCED_FACE('',(#809),#568,.T.);
#4997=ADVANCED_FACE('',(#810),#569,.T.);
#4998=ADVANCED_FACE('',(#811),#570,.T.);
#4999=ADVANCED_FACE('',(#812),#571,.T.);
#5000=ADVANCED_FACE('',(#813),#572,.T.);
#5001=ADVANCED_FACE('',(#814),#573,.T.);
#5002=ADVANCED_FACE('',(#815,#460,#461,#462,#463,#464),#574,.T.);
#5003=ADVANCED_FACE('',(#816,#465,#466),#575,.F.);
#5004=ADVANCED_FACE('',(#817),#4859,.F.);
#5005=ADVANCED_FACE('',(#818),#4860,.F.);
#5006=ADVANCED_FACE('',(#819),#576,.T.);
#5007=ADVANCED_FACE('',(#820,#467),#577,.T.);
#5008=ADVANCED_FACE('',(#821,#468),#578,.T.);
#5009=ADVANCED_FACE('',(#822),#579,.T.);
#5010=ADVANCED_FACE('',(#823),#580,.T.);
#5011=ADVANCED_FACE('',(#824),#581,.T.);
#5012=ADVANCED_FACE('',(#825,#469),#582,.T.);
#5013=ADVANCED_FACE('',(#826,#470),#583,.F.);
#5014=ADVANCED_FACE('',(#827),#4861,.F.);
#5015=ADVANCED_FACE('',(#828),#4862,.F.);
#5016=ADVANCED_FACE('',(#829),#584,.F.);
#5017=ADVANCED_FACE('',(#830,#471),#585,.F.);
#5018=ADVANCED_FACE('',(#831),#586,.T.);
#5019=ADVANCED_FACE('',(#832),#587,.T.);
#5020=ADVANCED_FACE('',(#833),#588,.T.);
#5021=ADVANCED_FACE('',(#834,#472),#589,.T.);
#5022=ADVANCED_FACE('',(#835),#4863,.F.);
#5023=ADVANCED_FACE('',(#836),#4864,.F.);
#5024=ADVANCED_FACE('',(#837),#4865,.F.);
#5025=ADVANCED_FACE('',(#838),#590,.T.);
#5026=ADVANCED_FACE('',(#839),#591,.T.);
#5027=ADVANCED_FACE('',(#840),#592,.F.);
#5028=ADVANCED_FACE('',(#841),#4866,.F.);
#5029=ADVANCED_FACE('',(#842),#4867,.F.);
#5030=ADVANCED_FACE('',(#843),#593,.T.);
#5031=ADVANCED_FACE('',(#844),#594,.T.);
#5032=ADVANCED_FACE('',(#845),#595,.T.);
#5033=ADVANCED_FACE('',(#846),#596,.T.);
#5034=ADVANCED_FACE('',(#847),#597,.T.);
#5035=ADVANCED_FACE('',(#848),#598,.T.);
#5036=ADVANCED_FACE('',(#849,#473,#474,#475,#476,#477),#599,.T.);
#5037=ADVANCED_FACE('',(#850,#478,#479),#600,.F.);
#5038=ADVANCED_FACE('',(#851),#4868,.F.);
#5039=ADVANCED_FACE('',(#852),#4869,.F.);
#5040=ADVANCED_FACE('',(#853),#601,.T.);
#5041=ADVANCED_FACE('',(#854,#480),#602,.T.);
#5042=ADVANCED_FACE('',(#855,#481),#603,.T.);
#5043=ADVANCED_FACE('',(#856),#604,.T.);
#5044=ADVANCED_FACE('',(#857),#605,.T.);
#5045=ADVANCED_FACE('',(#858),#606,.T.);
#5046=ADVANCED_FACE('',(#859,#482),#607,.T.);
#5047=ADVANCED_FACE('',(#860,#483),#608,.F.);
#5048=ADVANCED_FACE('',(#861),#609,.F.);
#5049=ADVANCED_FACE('',(#862),#610,.F.);
#5050=ADVANCED_FACE('',(#863),#611,.F.);
#5051=ADVANCED_FACE('',(#864),#612,.F.);
#5052=ADVANCED_FACE('',(#865),#613,.F.);
#5053=ADVANCED_FACE('',(#866),#614,.F.);
#5054=ADVANCED_FACE('',(#867),#615,.F.);
#5055=ADVANCED_FACE('',(#868),#616,.F.);
#5056=ADVANCED_FACE('',(#869),#617,.F.);
#5057=ADVANCED_FACE('',(#870),#618,.F.);
#5058=ADVANCED_FACE('',(#871),#619,.F.);
#5059=ADVANCED_FACE('',(#872),#620,.F.);
#5060=ADVANCED_FACE('',(#873),#621,.F.);
#5061=ADVANCED_FACE('',(#874),#622,.F.);
#5062=ADVANCED_FACE('',(#875),#623,.F.);
#5063=ADVANCED_FACE('',(#876),#624,.F.);
#5064=ADVANCED_FACE('',(#877),#625,.F.);
#5065=ADVANCED_FACE('',(#878),#626,.F.);
#5066=ADVANCED_FACE('',(#879),#627,.F.);
#5067=ADVANCED_FACE('',(#880),#628,.F.);
#5068=ADVANCED_FACE('',(#881),#629,.F.);
#5069=ADVANCED_FACE('',(#882),#630,.F.);
#5070=ADVANCED_FACE('',(#883),#631,.F.);
#5071=ADVANCED_FACE('',(#884),#632,.F.);
#5072=ADVANCED_FACE('',(#885),#633,.F.);
#5073=ADVANCED_FACE('',(#886),#634,.F.);
#5074=ADVANCED_FACE('',(#887),#635,.F.);
#5075=ADVANCED_FACE('',(#888),#636,.F.);
#5076=ADVANCED_FACE('',(#889),#637,.F.);
#5077=ADVANCED_FACE('',(#890),#638,.F.);
#5078=ADVANCED_FACE('',(#891),#639,.F.);
#5079=ADVANCED_FACE('',(#892),#640,.F.);
#5080=ADVANCED_FACE('',(#893),#641,.F.);
#5081=ADVANCED_FACE('',(#894),#642,.F.);
#5082=ADVANCED_FACE('',(#895),#643,.F.);
#5083=ADVANCED_FACE('',(#896),#644,.F.);
#5084=ADVANCED_FACE('',(#897),#4870,.F.);
#5085=ADVANCED_FACE('',(#898),#645,.T.);
#5086=ADVANCED_FACE('',(#899),#646,.T.);
#5087=ADVANCED_FACE('',(#900),#647,.T.);
#5088=ADVANCED_FACE('',(#901),#648,.T.);
#5089=ADVANCED_FACE('',(#902),#649,.T.);
#5090=ADVANCED_FACE('',(#903),#650,.T.);
#5091=ADVANCED_FACE('',(#904),#651,.T.);
#5092=ADVANCED_FACE('',(#905),#652,.T.);
#5093=ADVANCED_FACE('',(#906,#484),#653,.T.);
#5094=ADVANCED_FACE('',(#907,#485),#654,.F.);
#5095=ADVANCED_FACE('',(#908),#655,.T.);
#5096=ADVANCED_FACE('',(#909),#4871,.F.);
#5097=ADVANCED_FACE('',(#910),#656,.F.);
#5098=ADVANCED_FACE('',(#911),#657,.F.);
#5099=ADVANCED_FACE('',(#912),#658,.T.);
#5100=ADVANCED_FACE('',(#913),#659,.T.);
#5101=ADVANCED_FACE('',(#914),#660,.T.);
#5102=ADVANCED_FACE('',(#915),#661,.T.);
#5103=ADVANCED_FACE('',(#916),#662,.T.);
#5104=ADVANCED_FACE('',(#917,#486),#663,.T.);
#5105=ADVANCED_FACE('',(#918),#309,.F.);
#5106=ADVANCED_FACE('',(#919),#4872,.F.);
#5107=ADVANCED_FACE('',(#920,#487),#664,.T.);
#5108=ADVANCED_FACE('',(#921),#4873,.T.);
#5109=ADVANCED_FACE('',(#922,#488),#665,.F.);
#5110=ADVANCED_FACE('',(#923),#666,.F.);
#5111=ADVANCED_FACE('',(#924),#667,.F.);
#5112=ADVANCED_FACE('',(#925),#668,.F.);
#5113=ADVANCED_FACE('',(#926),#669,.F.);
#5114=ADVANCED_FACE('',(#927),#670,.F.);
#5115=ADVANCED_FACE('',(#928),#671,.F.);
#5116=ADVANCED_FACE('',(#929),#672,.F.);
#5117=ADVANCED_FACE('',(#930),#673,.F.);
#5118=ADVANCED_FACE('',(#931),#674,.F.);
#5119=ADVANCED_FACE('',(#932),#675,.T.);
#5120=ADVANCED_FACE('',(#933),#310,.T.);
#5121=ADVANCED_FACE('',(#934),#4874,.T.);
#5122=ADVANCED_FACE('',(#935),#311,.T.);
#5123=ADVANCED_FACE('',(#936,#489),#676,.T.);
#5124=ADVANCED_FACE('',(#937),#312,.T.);
#5125=ADVANCED_FACE('',(#938),#4875,.T.);
#5126=ADVANCED_FACE('',(#939),#4876,.T.);
#5127=ADVANCED_FACE('',(#940),#313,.T.);
#5128=ADVANCED_FACE('',(#941),#677,.T.);
#5129=ADVANCED_FACE('',(#942),#314,.T.);
#5130=ADVANCED_FACE('',(#943),#678,.T.);
#5131=ADVANCED_FACE('',(#944),#679,.T.);
#5132=ADVANCED_FACE('',(#945),#680,.T.);
#5133=ADVANCED_FACE('',(#946),#681,.T.);
#5134=ADVANCED_FACE('',(#947),#682,.T.);
#5135=ADVANCED_FACE('',(#948),#683,.T.);
#5136=ADVANCED_FACE('',(#949),#684,.T.);
#5137=ADVANCED_FACE('',(#950,#490),#685,.F.);
#5138=ADVANCED_FACE('',(#951),#315,.T.);
#5139=ADVANCED_FACE('',(#952),#316,.T.);
#5140=ADVANCED_FACE('',(#953),#686,.T.);
#5141=ADVANCED_FACE('',(#954),#687,.T.);
#5142=ADVANCED_FACE('',(#955),#688,.T.);
#5143=ADVANCED_FACE('',(#956),#4877,.F.);
#5144=ADVANCED_FACE('',(#957),#689,.T.);
#5145=ADVANCED_FACE('',(#958),#690,.T.);
#5146=ADVANCED_FACE('',(#959),#691,.T.);
#5147=ADVANCED_FACE('',(#960,#491),#692,.T.);
#5148=ADVANCED_FACE('',(#961,#492),#693,.F.);
#5149=ADVANCED_FACE('',(#962),#4878,.F.);
#5150=ADVANCED_FACE('',(#963),#4879,.F.);
#5151=ADVANCED_FACE('',(#964),#4880,.F.);
#5152=ADVANCED_FACE('',(#965),#4881,.F.);
#5153=ADVANCED_FACE('',(#966),#4882,.F.);
#5154=ADVANCED_FACE('',(#967,#493),#694,.F.);
#5155=ADVANCED_FACE('',(#968),#4883,.F.);
#5156=ADVANCED_FACE('',(#969),#4884,.T.);
#5157=ADVANCED_FACE('',(#970,#494,#495,#496,#497,#498),#695,.T.);
#5158=ADVANCED_FACE('',(#971,#499,#500,#501,#502,#503),#696,.F.);
#5159=ADVANCED_FACE('',(#972),#4885,.F.);
#5160=ADVANCED_FACE('',(#973),#4886,.F.);
#5161=ADVANCED_FACE('',(#974),#4887,.F.);
#5162=ADVANCED_FACE('',(#975),#4888,.F.);
#5163=ADVANCED_FACE('',(#976),#4889,.F.);
#5164=ADVANCED_FACE('',(#977,#504),#697,.T.);
#5165=ADVANCED_FACE('',(#978),#4890,.F.);
#5166=ADVANCED_FACE('',(#979),#4891,.T.);
#5167=ADVANCED_FACE('',(#980,#505,#506,#507,#508,#509),#698,.T.);
#5168=ADVANCED_FACE('',(#981,#510,#511,#512,#513,#514),#699,.F.);
#5169=ADVANCED_FACE('',(#982),#4892,.F.);
#5170=ADVANCED_FACE('',(#983),#4893,.T.);
#5171=ADVANCED_FACE('',(#984,#515),#700,.T.);
#5172=ADVANCED_FACE('',(#985,#516),#701,.F.);
#5173=ADVANCED_FACE('',(#986),#4894,.F.);
#5174=ADVANCED_FACE('',(#987),#4895,.F.);
#5175=ADVANCED_FACE('',(#988),#4896,.F.);
#5176=ADVANCED_FACE('',(#989),#4897,.F.);
#5177=ADVANCED_FACE('',(#990),#4898,.F.);
#5178=ADVANCED_FACE('',(#991),#4899,.T.);
#5179=ADVANCED_FACE('',(#992,#517,#518,#519,#520,#521),#702,.T.);
#5180=ADVANCED_FACE('',(#993,#522,#523,#524,#525,#526),#703,.F.);
#5181=ADVANCED_FACE('',(#994),#704,.T.);
#5182=ADVANCED_FACE('',(#995),#317,.T.);
#5183=ADVANCED_FACE('',(#996),#4900,.T.);
#5184=ADVANCED_FACE('',(#997),#318,.T.);
#5185=ADVANCED_FACE('',(#998,#527),#705,.T.);
#5186=ADVANCED_FACE('',(#999),#319,.T.);
#5187=ADVANCED_FACE('',(#1000),#4901,.T.);
#5188=ADVANCED_FACE('',(#1001),#320,.T.);
#5189=ADVANCED_FACE('',(#1002),#706,.T.);
#5190=ADVANCED_FACE('',(#1003),#707,.F.);
#5191=ADVANCED_FACE('',(#1004),#708,.F.);
#5192=ADVANCED_FACE('',(#1005),#709,.F.);
#5193=ADVANCED_FACE('',(#1006),#710,.F.);
#5194=ADVANCED_FACE('',(#1007),#711,.F.);
#5195=ADVANCED_FACE('',(#1008),#712,.F.);
#5196=ADVANCED_FACE('',(#1009),#713,.F.);
#5197=ADVANCED_FACE('',(#1010),#714,.F.);
#5198=CLOSED_SHELL('',(#4902,#4903,#4904,#4905,#4906,#4907,#4908,#4909,
#4910,#4911,#4912));
#5199=CLOSED_SHELL('',(#4913,#4914,#4915,#4916));
#5200=CLOSED_SHELL('',(#4917,#4918,#4919,#4920));
#5201=CLOSED_SHELL('',(#4921,#4922,#4923,#4924));
#5202=CLOSED_SHELL('',(#4925,#4926,#4927,#4928));
#5203=CLOSED_SHELL('',(#4929,#4930,#4931,#4932,#4933,#4934,#4935,#4936));
#5204=CLOSED_SHELL('',(#4937,#4938,#4939,#4940,#4941,#4942,#4943,#4944));
#5205=CLOSED_SHELL('',(#4945));
#5206=CLOSED_SHELL('',(#4946));
#5207=CLOSED_SHELL('',(#4947));
#5208=CLOSED_SHELL('',(#4948));
#5209=CLOSED_SHELL('',(#4949));
#5210=CLOSED_SHELL('',(#4950));
#5211=CLOSED_SHELL('',(#4951));
#5212=CLOSED_SHELL('',(#4952));
#5213=CLOSED_SHELL('',(#4953,#4954,#4955,#4956,#4957,#4958,#4959,#4960,
#4961,#4962,#4963,#4964,#4965,#4966,#4967,#4968,#4969,#4970,#4971));
#5214=CLOSED_SHELL('',(#4972,#4973,#4974,#4975));
#5215=CLOSED_SHELL('',(#4976,#4977,#4978,#4979));
#5216=CLOSED_SHELL('',(#4980,#4981,#4982,#4983,#4984,#4985,#4986,#4987,
#4988,#4989,#4990,#4991,#4992,#4993,#4994,#4995,#4996,#4997,#4998,#4999,
#5000,#5001,#5002,#5003));
#5217=CLOSED_SHELL('',(#5004,#5005,#5006,#5007,#5008,#5009,#5010,#5011,
#5012,#5013));
#5218=CLOSED_SHELL('',(#5014,#5015,#5016,#5017,#5018,#5019,#5020,#5021,
#5022,#5023,#5024,#5025,#5026,#5027,#5028,#5029,#5030,#5031,#5032,#5033,
#5034,#5035,#5036,#5037));
#5219=CLOSED_SHELL('',(#5038,#5039,#5040,#5041,#5042,#5043,#5044,#5045,
#5046,#5047));
#5220=CLOSED_SHELL('',(#5048,#5049,#5050,#5051,#5052,#5053,#5054,#5055,
#5056,#5057,#5058,#5059,#5060,#5061,#5062,#5063,#5064,#5065,#5066,#5067,
#5068,#5069,#5070,#5071,#5072,#5073,#5074,#5075,#5076,#5077,#5078,#5079,
#5080,#5081,#5082,#5083,#5084,#5085,#5086,#5087,#5088,#5089,#5090,#5091,
#5092,#5093,#5094));
#5221=CLOSED_SHELL('',(#5095,#5096,#5097,#5098,#5099,#5100,#5101,#5102,
#5103,#5104));
#5222=CLOSED_SHELL('',(#5105,#5106,#5107,#5108,#5109));
#5223=CLOSED_SHELL('',(#5110,#5111,#5112,#5113,#5114,#5115,#5116,#5117));
#5224=CLOSED_SHELL('',(#5118,#5119,#5120,#5121,#5122,#5123,#5124,#5125));
#5225=CLOSED_SHELL('',(#5126,#5127,#5128,#5129,#5130,#5131,#5132,#5133,
#5134,#5135,#5136,#5137));
#5226=CLOSED_SHELL('',(#5138,#5139,#5140,#5141,#5142,#5143,#5144,#5145,
#5146,#5147,#5148));
#5227=CLOSED_SHELL('',(#5149,#5150,#5151,#5152,#5153,#5154,#5155,#5156,
#5157,#5158));
#5228=CLOSED_SHELL('',(#5159,#5160,#5161,#5162,#5163,#5164,#5165,#5166,
#5167,#5168));
#5229=CLOSED_SHELL('',(#5169,#5170,#5171,#5172));
#5230=CLOSED_SHELL('',(#5173,#5174,#5175,#5176,#5177,#5178,#5179,#5180));
#5231=CLOSED_SHELL('',(#5181,#5182,#5183,#5184,#5185,#5186,#5187,#5188,
#5189));
#5232=CLOSED_SHELL('',(#5190,#5191,#5192,#5193,#5194,#5195,#5196,#5197));
#5233=DERIVED_UNIT_ELEMENT(#5283,1.);
#5234=DERIVED_UNIT_ELEMENT(#9624,-3.);
#5235=DERIVED_UNIT_ELEMENT(#5283,1.);
#5236=DERIVED_UNIT_ELEMENT(#9624,-3.);
#5237=DERIVED_UNIT_ELEMENT(#5283,1.);
#5238=DERIVED_UNIT_ELEMENT(#9624,-3.);
#5239=DERIVED_UNIT_ELEMENT(#5283,1.);
#5240=DERIVED_UNIT_ELEMENT(#9624,-3.);
#5241=DERIVED_UNIT_ELEMENT(#5283,1.);
#5242=DERIVED_UNIT_ELEMENT(#9624,-3.);
#5243=DERIVED_UNIT_ELEMENT(#5283,1.);
#5244=DERIVED_UNIT_ELEMENT(#9624,-3.);
#5245=DERIVED_UNIT_ELEMENT(#5283,1.);
#5246=DERIVED_UNIT_ELEMENT(#9624,-3.);
#5247=DERIVED_UNIT_ELEMENT(#5283,1.);
#5248=DERIVED_UNIT_ELEMENT(#9624,-3.);
#5249=DERIVED_UNIT_ELEMENT(#5283,1.);
#5250=DERIVED_UNIT_ELEMENT(#9624,-3.);
#5251=DERIVED_UNIT_ELEMENT(#5283,1.);
#5252=DERIVED_UNIT_ELEMENT(#9624,-3.);
#5253=DERIVED_UNIT_ELEMENT(#5283,1.);
#5254=DERIVED_UNIT_ELEMENT(#9624,-3.);
#5255=DERIVED_UNIT_ELEMENT(#5283,1.);
#5256=DERIVED_UNIT_ELEMENT(#9624,-3.);
#5257=DERIVED_UNIT_ELEMENT(#5283,1.);
#5258=DERIVED_UNIT_ELEMENT(#9624,-3.);
#5259=DERIVED_UNIT_ELEMENT(#5283,1.);
#5260=DERIVED_UNIT_ELEMENT(#9624,-3.);
#5261=DERIVED_UNIT_ELEMENT(#5283,1.);
#5262=DERIVED_UNIT_ELEMENT(#9624,-3.);
#5263=DERIVED_UNIT_ELEMENT(#5283,1.);
#5264=DERIVED_UNIT_ELEMENT(#9624,-3.);
#5265=DERIVED_UNIT_ELEMENT(#5283,1.);
#5266=DERIVED_UNIT_ELEMENT(#9624,-3.);
#5267=DERIVED_UNIT_ELEMENT(#5283,1.);
#5268=DERIVED_UNIT_ELEMENT(#9624,-3.);
#5269=DERIVED_UNIT_ELEMENT(#5283,1.);
#5270=DERIVED_UNIT_ELEMENT(#9624,-3.);
#5271=DERIVED_UNIT_ELEMENT(#5283,1.);
#5272=DERIVED_UNIT_ELEMENT(#9624,-3.);
#5273=DERIVED_UNIT_ELEMENT(#5283,1.);
#5274=DERIVED_UNIT_ELEMENT(#9624,-3.);
#5275=DERIVED_UNIT_ELEMENT(#5283,1.);
#5276=DERIVED_UNIT_ELEMENT(#9624,-3.);
#5277=DERIVED_UNIT_ELEMENT(#5283,1.);
#5278=DERIVED_UNIT_ELEMENT(#9624,-3.);
#5279=DERIVED_UNIT_ELEMENT(#5283,1.);
#5280=DERIVED_UNIT_ELEMENT(#9624,-3.);
#5281=DERIVED_UNIT_ELEMENT(#5283,1.);
#5282=DERIVED_UNIT_ELEMENT(#9624,-3.);
#5283=(
MASS_UNIT()
NAMED_UNIT(*)
SI_UNIT(.KILO.,.GRAM.)
);
#5284=DERIVED_UNIT((#5233,#5234));
#5285=DERIVED_UNIT((#5235,#5236));
#5286=DERIVED_UNIT((#5237,#5238));
#5287=DERIVED_UNIT((#5239,#5240));
#5288=DERIVED_UNIT((#5241,#5242));
#5289=DERIVED_UNIT((#5243,#5244));
#5290=DERIVED_UNIT((#5245,#5246));
#5291=DERIVED_UNIT((#5247,#5248));
#5292=DERIVED_UNIT((#5249,#5250));
#5293=DERIVED_UNIT((#5251,#5252));
#5294=DERIVED_UNIT((#5253,#5254));
#5295=DERIVED_UNIT((#5255,#5256));
#5296=DERIVED_UNIT((#5257,#5258));
#5297=DERIVED_UNIT((#5259,#5260));
#5298=DERIVED_UNIT((#5261,#5262));
#5299=DERIVED_UNIT((#5263,#5264));
#5300=DERIVED_UNIT((#5265,#5266));
#5301=DERIVED_UNIT((#5267,#5268));
#5302=DERIVED_UNIT((#5269,#5270));
#5303=DERIVED_UNIT((#5271,#5272));
#5304=DERIVED_UNIT((#5273,#5274));
#5305=DERIVED_UNIT((#5275,#5276));
#5306=DERIVED_UNIT((#5277,#5278));
#5307=DERIVED_UNIT((#5279,#5280));
#5308=DERIVED_UNIT((#5281,#5282));
#5309=MEASURE_REPRESENTATION_ITEM('density measure',
POSITIVE_RATIO_MEASURE(7850.),#5284);
#5310=MEASURE_REPRESENTATION_ITEM('density measure',
POSITIVE_RATIO_MEASURE(7850.),#5285);
#5311=MEASURE_REPRESENTATION_ITEM('density measure',
POSITIVE_RATIO_MEASURE(7850.),#5286);
#5312=MEASURE_REPRESENTATION_ITEM('density measure',
POSITIVE_RATIO_MEASURE(7850.),#5287);
#5313=MEASURE_REPRESENTATION_ITEM('density measure',
POSITIVE_RATIO_MEASURE(7850.),#5288);
#5314=MEASURE_REPRESENTATION_ITEM('density measure',
POSITIVE_RATIO_MEASURE(7850.),#5289);
#5315=MEASURE_REPRESENTATION_ITEM('density measure',
POSITIVE_RATIO_MEASURE(7850.),#5290);
#5316=MEASURE_REPRESENTATION_ITEM('density measure',
POSITIVE_RATIO_MEASURE(7850.),#5291);
#5317=MEASURE_REPRESENTATION_ITEM('density measure',
POSITIVE_RATIO_MEASURE(7850.),#5292);
#5318=MEASURE_REPRESENTATION_ITEM('density measure',
POSITIVE_RATIO_MEASURE(7850.),#5293);
#5319=MEASURE_REPRESENTATION_ITEM('density measure',
POSITIVE_RATIO_MEASURE(7850.),#5294);
#5320=MEASURE_REPRESENTATION_ITEM('density measure',
POSITIVE_RATIO_MEASURE(7850.),#5295);
#5321=MEASURE_REPRESENTATION_ITEM('density measure',
POSITIVE_RATIO_MEASURE(7850.),#5296);
#5322=MEASURE_REPRESENTATION_ITEM('density measure',
POSITIVE_RATIO_MEASURE(7850.),#5297);
#5323=MEASURE_REPRESENTATION_ITEM('density measure',
POSITIVE_RATIO_MEASURE(7850.),#5298);
#5324=MEASURE_REPRESENTATION_ITEM('density measure',
POSITIVE_RATIO_MEASURE(7850.),#5299);
#5325=MEASURE_REPRESENTATION_ITEM('density measure',
POSITIVE_RATIO_MEASURE(7850.),#5300);
#5326=MEASURE_REPRESENTATION_ITEM('density measure',
POSITIVE_RATIO_MEASURE(7850.),#5301);
#5327=MEASURE_REPRESENTATION_ITEM('density measure',
POSITIVE_RATIO_MEASURE(7850.),#5302);
#5328=MEASURE_REPRESENTATION_ITEM('density measure',
POSITIVE_RATIO_MEASURE(7850.),#5303);
#5329=MEASURE_REPRESENTATION_ITEM('density measure',
POSITIVE_RATIO_MEASURE(7850.),#5304);
#5330=MEASURE_REPRESENTATION_ITEM('density measure',
POSITIVE_RATIO_MEASURE(7850.),#5305);
#5331=MEASURE_REPRESENTATION_ITEM('density measure',
POSITIVE_RATIO_MEASURE(7850.),#5306);
#5332=MEASURE_REPRESENTATION_ITEM('density measure',
POSITIVE_RATIO_MEASURE(7850.),#5307);
#5333=MEASURE_REPRESENTATION_ITEM('density measure',
POSITIVE_RATIO_MEASURE(7850.),#5308);
#5334=PROPERTY_DEFINITION_REPRESENTATION(#5459,#5384);
#5335=PROPERTY_DEFINITION_REPRESENTATION(#5460,#5385);
#5336=PROPERTY_DEFINITION_REPRESENTATION(#5461,#5386);
#5337=PROPERTY_DEFINITION_REPRESENTATION(#5462,#5387);
#5338=PROPERTY_DEFINITION_REPRESENTATION(#5463,#5388);
#5339=PROPERTY_DEFINITION_REPRESENTATION(#5464,#5389);
#5340=PROPERTY_DEFINITION_REPRESENTATION(#5465,#5390);
#5341=PROPERTY_DEFINITION_REPRESENTATION(#5466,#5391);
#5342=PROPERTY_DEFINITION_REPRESENTATION(#5467,#5392);
#5343=PROPERTY_DEFINITION_REPRESENTATION(#5468,#5393);
#5344=PROPERTY_DEFINITION_REPRESENTATION(#5469,#5394);
#5345=PROPERTY_DEFINITION_REPRESENTATION(#5470,#5395);
#5346=PROPERTY_DEFINITION_REPRESENTATION(#5471,#5396);
#5347=PROPERTY_DEFINITION_REPRESENTATION(#5472,#5397);
#5348=PROPERTY_DEFINITION_REPRESENTATION(#5473,#5398);
#5349=PROPERTY_DEFINITION_REPRESENTATION(#5474,#5399);
#5350=PROPERTY_DEFINITION_REPRESENTATION(#5475,#5400);
#5351=PROPERTY_DEFINITION_REPRESENTATION(#5476,#5401);
#5352=PROPERTY_DEFINITION_REPRESENTATION(#5477,#5402);
#5353=PROPERTY_DEFINITION_REPRESENTATION(#5478,#5403);
#5354=PROPERTY_DEFINITION_REPRESENTATION(#5479,#5404);
#5355=PROPERTY_DEFINITION_REPRESENTATION(#5480,#5405);
#5356=PROPERTY_DEFINITION_REPRESENTATION(#5481,#5406);
#5357=PROPERTY_DEFINITION_REPRESENTATION(#5482,#5407);
#5358=PROPERTY_DEFINITION_REPRESENTATION(#5483,#5408);
#5359=PROPERTY_DEFINITION_REPRESENTATION(#5484,#5409);
#5360=PROPERTY_DEFINITION_REPRESENTATION(#5485,#5410);
#5361=PROPERTY_DEFINITION_REPRESENTATION(#5486,#5411);
#5362=PROPERTY_DEFINITION_REPRESENTATION(#5487,#5412);
#5363=PROPERTY_DEFINITION_REPRESENTATION(#5488,#5413);
#5364=PROPERTY_DEFINITION_REPRESENTATION(#5489,#5414);
#5365=PROPERTY_DEFINITION_REPRESENTATION(#5490,#5415);
#5366=PROPERTY_DEFINITION_REPRESENTATION(#5491,#5416);
#5367=PROPERTY_DEFINITION_REPRESENTATION(#5492,#5417);
#5368=PROPERTY_DEFINITION_REPRESENTATION(#5493,#5418);
#5369=PROPERTY_DEFINITION_REPRESENTATION(#5494,#5419);
#5370=PROPERTY_DEFINITION_REPRESENTATION(#5495,#5420);
#5371=PROPERTY_DEFINITION_REPRESENTATION(#5496,#5421);
#5372=PROPERTY_DEFINITION_REPRESENTATION(#5497,#5422);
#5373=PROPERTY_DEFINITION_REPRESENTATION(#5498,#5423);
#5374=PROPERTY_DEFINITION_REPRESENTATION(#5499,#5424);
#5375=PROPERTY_DEFINITION_REPRESENTATION(#5500,#5425);
#5376=PROPERTY_DEFINITION_REPRESENTATION(#5501,#5426);
#5377=PROPERTY_DEFINITION_REPRESENTATION(#5502,#5427);
#5378=PROPERTY_DEFINITION_REPRESENTATION(#5503,#5428);
#5379=PROPERTY_DEFINITION_REPRESENTATION(#5504,#5429);
#5380=PROPERTY_DEFINITION_REPRESENTATION(#5505,#5430);
#5381=PROPERTY_DEFINITION_REPRESENTATION(#5506,#5431);
#5382=PROPERTY_DEFINITION_REPRESENTATION(#5507,#5432);
#5383=PROPERTY_DEFINITION_REPRESENTATION(#5508,#5433);
#5384=REPRESENTATION('material name',(#5434),#9595);
#5385=REPRESENTATION('density',(#5309),#9595);
#5386=REPRESENTATION('material name',(#5435),#9596);
#5387=REPRESENTATION('density',(#5310),#9596);
#5388=REPRESENTATION('material name',(#5436),#9597);
#5389=REPRESENTATION('density',(#5311),#9597);
#5390=REPRESENTATION('material name',(#5437),#9598);
#5391=REPRESENTATION('density',(#5312),#9598);
#5392=REPRESENTATION('material name',(#5438),#9599);
#5393=REPRESENTATION('density',(#5313),#9599);
#5394=REPRESENTATION('material name',(#5439),#9601);
#5395=REPRESENTATION('density',(#5314),#9601);
#5396=REPRESENTATION('material name',(#5440),#9602);
#5397=REPRESENTATION('density',(#5315),#9602);
#5398=REPRESENTATION('material name',(#5441),#9603);
#5399=REPRESENTATION('density',(#5316),#9603);
#5400=REPRESENTATION('material name',(#5442),#9604);
#5401=REPRESENTATION('density',(#5317),#9604);
#5402=REPRESENTATION('material name',(#5443),#9605);
#5403=REPRESENTATION('density',(#5318),#9605);
#5404=REPRESENTATION('material name',(#5444),#9606);
#5405=REPRESENTATION('density',(#5319),#9606);
#5406=REPRESENTATION('material name',(#5445),#9607);
#5407=REPRESENTATION('density',(#5320),#9607);
#5408=REPRESENTATION('material name',(#5446),#9608);
#5409=REPRESENTATION('density',(#5321),#9608);
#5410=REPRESENTATION('material name',(#5447),#9609);
#5411=REPRESENTATION('density',(#5322),#9609);
#5412=REPRESENTATION('material name',(#5448),#9610);
#5413=REPRESENTATION('density',(#5323),#9610);
#5414=REPRESENTATION('material name',(#5449),#9611);
#5415=REPRESENTATION('density',(#5324),#9611);
#5416=REPRESENTATION('material name',(#5450),#9612);
#5417=REPRESENTATION('density',(#5325),#9612);
#5418=REPRESENTATION('material name',(#5451),#9613);
#5419=REPRESENTATION('density',(#5326),#9613);
#5420=REPRESENTATION('material name',(#5452),#9614);
#5421=REPRESENTATION('density',(#5327),#9614);
#5422=REPRESENTATION('material name',(#5453),#9615);
#5423=REPRESENTATION('density',(#5328),#9615);
#5424=REPRESENTATION('material name',(#5454),#9617);
#5425=REPRESENTATION('density',(#5329),#9617);
#5426=REPRESENTATION('material name',(#5455),#9618);
#5427=REPRESENTATION('density',(#5330),#9618);
#5428=REPRESENTATION('material name',(#5456),#9619);
#5429=REPRESENTATION('density',(#5331),#9619);
#5430=REPRESENTATION('material name',(#5457),#9620);
#5431=REPRESENTATION('density',(#5332),#9620);
#5432=REPRESENTATION('material name',(#5458),#9621);
#5433=REPRESENTATION('density',(#5333),#9621);
#5434=DESCRIPTIVE_REPRESENTATION_ITEM('Steel','Steel');
#5435=DESCRIPTIVE_REPRESENTATION_ITEM('Steel','Steel');
#5436=DESCRIPTIVE_REPRESENTATION_ITEM('Steel','Steel');
#5437=DESCRIPTIVE_REPRESENTATION_ITEM('Steel','Steel');
#5438=DESCRIPTIVE_REPRESENTATION_ITEM('Steel','Steel');
#5439=DESCRIPTIVE_REPRESENTATION_ITEM('Steel','Steel');
#5440=DESCRIPTIVE_REPRESENTATION_ITEM('Steel','Steel');
#5441=DESCRIPTIVE_REPRESENTATION_ITEM('Steel','Steel');
#5442=DESCRIPTIVE_REPRESENTATION_ITEM('Steel','Steel');
#5443=DESCRIPTIVE_REPRESENTATION_ITEM('Steel','Steel');
#5444=DESCRIPTIVE_REPRESENTATION_ITEM('Steel','Steel');
#5445=DESCRIPTIVE_REPRESENTATION_ITEM('Steel','Steel');
#5446=DESCRIPTIVE_REPRESENTATION_ITEM('Steel','Steel');
#5447=DESCRIPTIVE_REPRESENTATION_ITEM('Steel','Steel');
#5448=DESCRIPTIVE_REPRESENTATION_ITEM('Steel','Steel');
#5449=DESCRIPTIVE_REPRESENTATION_ITEM('Steel','Steel');
#5450=DESCRIPTIVE_REPRESENTATION_ITEM('Steel','Steel');
#5451=DESCRIPTIVE_REPRESENTATION_ITEM('Steel','Steel');
#5452=DESCRIPTIVE_REPRESENTATION_ITEM('Steel','Steel');
#5453=DESCRIPTIVE_REPRESENTATION_ITEM('Steel','Steel');
#5454=DESCRIPTIVE_REPRESENTATION_ITEM('Steel','Steel');
#5455=DESCRIPTIVE_REPRESENTATION_ITEM('Steel','Steel');
#5456=DESCRIPTIVE_REPRESENTATION_ITEM('Steel','Steel');
#5457=DESCRIPTIVE_REPRESENTATION_ITEM('Steel','Steel');
#5458=DESCRIPTIVE_REPRESENTATION_ITEM('Steel','Steel');
#5459=PROPERTY_DEFINITION('material property','material name',#9776);
#5460=PROPERTY_DEFINITION('material property','density of part',#9776);
#5461=PROPERTY_DEFINITION('material property','material name',#9777);
#5462=PROPERTY_DEFINITION('material property','density of part',#9777);
#5463=PROPERTY_DEFINITION('material property','material name',#9778);
#5464=PROPERTY_DEFINITION('material property','density of part',#9778);
#5465=PROPERTY_DEFINITION('material property','material name',#9779);
#5466=PROPERTY_DEFINITION('material property','density of part',#9779);
#5467=PROPERTY_DEFINITION('material property','material name',#9780);
#5468=PROPERTY_DEFINITION('material property','density of part',#9780);
#5469=PROPERTY_DEFINITION('material property','material name',#9782);
#5470=PROPERTY_DEFINITION('material property','density of part',#9782);
#5471=PROPERTY_DEFINITION('material property','material name',#9783);
#5472=PROPERTY_DEFINITION('material property','density of part',#9783);
#5473=PROPERTY_DEFINITION('material property','material name',#9784);
#5474=PROPERTY_DEFINITION('material property','density of part',#9784);
#5475=PROPERTY_DEFINITION('material property','material name',#9785);
#5476=PROPERTY_DEFINITION('material property','density of part',#9785);
#5477=PROPERTY_DEFINITION('material property','material name',#9786);
#5478=PROPERTY_DEFINITION('material property','density of part',#9786);
#5479=PROPERTY_DEFINITION('material property','material name',#9787);
#5480=PROPERTY_DEFINITION('material property','density of part',#9787);
#5481=PROPERTY_DEFINITION('material property','material name',#9788);
#5482=PROPERTY_DEFINITION('material property','density of part',#9788);
#5483=PROPERTY_DEFINITION('material property','material name',#9789);
#5484=PROPERTY_DEFINITION('material property','density of part',#9789);
#5485=PROPERTY_DEFINITION('material property','material name',#9790);
#5486=PROPERTY_DEFINITION('material property','density of part',#9790);
#5487=PROPERTY_DEFINITION('material property','material name',#9791);
#5488=PROPERTY_DEFINITION('material property','density of part',#9791);
#5489=PROPERTY_DEFINITION('material property','material name',#9792);
#5490=PROPERTY_DEFINITION('material property','density of part',#9792);
#5491=PROPERTY_DEFINITION('material property','material name',#9793);
#5492=PROPERTY_DEFINITION('material property','density of part',#9793);
#5493=PROPERTY_DEFINITION('material property','material name',#9794);
#5494=PROPERTY_DEFINITION('material property','density of part',#9794);
#5495=PROPERTY_DEFINITION('material property','material name',#9795);
#5496=PROPERTY_DEFINITION('material property','density of part',#9795);
#5497=PROPERTY_DEFINITION('material property','material name',#9796);
#5498=PROPERTY_DEFINITION('material property','density of part',#9796);
#5499=PROPERTY_DEFINITION('material property','material name',#9798);
#5500=PROPERTY_DEFINITION('material property','density of part',#9798);
#5501=PROPERTY_DEFINITION('material property','material name',#9799);
#5502=PROPERTY_DEFINITION('material property','density of part',#9799);
#5503=PROPERTY_DEFINITION('material property','material name',#9800);
#5504=PROPERTY_DEFINITION('material property','density of part',#9800);
#5505=PROPERTY_DEFINITION('material property','material name',#9801);
#5506=PROPERTY_DEFINITION('material property','density of part',#9801);
#5507=PROPERTY_DEFINITION('material property','material name',#9802);
#5508=PROPERTY_DEFINITION('material property','density of part',#9802);
#5509=AXIS2_PLACEMENT_3D('',#7708,#6107,#6108);
#5510=AXIS2_PLACEMENT_3D('',#7709,#6109,#6110);
#5511=AXIS2_PLACEMENT_3D('',#7710,#6111,#6112);
#5512=AXIS2_PLACEMENT_3D('',#7711,#6113,#6114);
#5513=AXIS2_PLACEMENT_3D('',#7713,#6115,#6116);
#5514=AXIS2_PLACEMENT_3D('',#7716,#6118,#6119);
#5515=AXIS2_PLACEMENT_3D('',#7717,#6120,#6121);
#5516=AXIS2_PLACEMENT_3D('',#7718,#6122,#6123);
#5517=AXIS2_PLACEMENT_3D('',#7720,#6124,#6125);
#5518=AXIS2_PLACEMENT_3D('',#7723,#6127,#6128);
#5519=AXIS2_PLACEMENT_3D('',#7724,#6129,#6130);
#5520=AXIS2_PLACEMENT_3D('',#7725,#6131,#6132);
#5521=AXIS2_PLACEMENT_3D('',#7727,#6133,#6134);
#5522=AXIS2_PLACEMENT_3D('',#7729,#6135,#6136);
#5523=AXIS2_PLACEMENT_3D('',#7730,#6137,#6138);
#5524=AXIS2_PLACEMENT_3D('',#7732,#6139,#6140);
#5525=AXIS2_PLACEMENT_3D('',#7734,#6141,#6142);
#5526=AXIS2_PLACEMENT_3D('',#7735,#6143,#6144);
#5527=AXIS2_PLACEMENT_3D('',#7737,#6146,#6147);
#5528=AXIS2_PLACEMENT_3D('',#7740,#6149,#6150);
#5529=AXIS2_PLACEMENT_3D('',#7741,#6151,#6152);
#5530=AXIS2_PLACEMENT_3D('',#7743,#6153,#6154);
#5531=AXIS2_PLACEMENT_3D('',#7745,#6156,#6157);
#5532=AXIS2_PLACEMENT_3D('',#7746,#6158,#6159);
#5533=AXIS2_PLACEMENT_3D('',#7747,#6160,#6161);
#5534=AXIS2_PLACEMENT_3D('',#7748,#6162,#6163);
#5535=AXIS2_PLACEMENT_3D('',#7750,#6164,#6165);
#5536=AXIS2_PLACEMENT_3D('',#7753,#6167,#6168);
#5537=AXIS2_PLACEMENT_3D('',#7754,#6169,#6170);
#5538=AXIS2_PLACEMENT_3D('',#7756,#6171,#6172);
#5539=AXIS2_PLACEMENT_3D('',#7759,#6174,#6175);
#5540=AXIS2_PLACEMENT_3D('',#7760,#6176,#6177);
#5541=AXIS2_PLACEMENT_3D('',#7761,#6178,#6179);
#5542=AXIS2_PLACEMENT_3D('',#7762,#6180,#6181);
#5543=AXIS2_PLACEMENT_3D('',#7763,#6182,#6183);
#5544=AXIS2_PLACEMENT_3D('',#7765,#6184,#6185);
#5545=AXIS2_PLACEMENT_3D('',#7768,#6187,#6188);
#5546=AXIS2_PLACEMENT_3D('',#7769,#6189,#6190);
#5547=AXIS2_PLACEMENT_3D('',#7771,#6191,#6192);
#5548=AXIS2_PLACEMENT_3D('',#7774,#6194,#6195);
#5549=AXIS2_PLACEMENT_3D('',#7775,#6196,#6197);
#5550=AXIS2_PLACEMENT_3D('',#7776,#6198,#6199);
#5551=AXIS2_PLACEMENT_3D('',#7777,#6200,#6201);
#5552=AXIS2_PLACEMENT_3D('',#7778,#6202,#6203);
#5553=AXIS2_PLACEMENT_3D('',#7780,#6204,#6205);
#5554=AXIS2_PLACEMENT_3D('',#7783,#6207,#6208);
#5555=AXIS2_PLACEMENT_3D('',#7784,#6209,#6210);
#5556=AXIS2_PLACEMENT_3D('',#7786,#6211,#6212);
#5557=AXIS2_PLACEMENT_3D('',#7789,#6214,#6215);
#5558=AXIS2_PLACEMENT_3D('',#7790,#6216,#6217);
#5559=AXIS2_PLACEMENT_3D('',#7791,#6218,#6219);
#5560=AXIS2_PLACEMENT_3D('',#7792,#6220,#6221);
#5561=AXIS2_PLACEMENT_3D('',#7793,#6222,#6223);
#5562=AXIS2_PLACEMENT_3D('',#7795,#6224,#6225);
#5563=AXIS2_PLACEMENT_3D('',#7798,#6227,#6228);
#5564=AXIS2_PLACEMENT_3D('',#7799,#6229,#6230);
#5565=AXIS2_PLACEMENT_3D('',#7801,#6231,#6232);
#5566=AXIS2_PLACEMENT_3D('',#7804,#6234,#6235);
#5567=AXIS2_PLACEMENT_3D('',#7805,#6236,#6237);
#5568=AXIS2_PLACEMENT_3D('',#7806,#6238,#6239);
#5569=AXIS2_PLACEMENT_3D('',#7807,#6240,#6241);
#5570=AXIS2_PLACEMENT_3D('',#7808,#6242,#6243);
#5571=AXIS2_PLACEMENT_3D('',#7809,#6244,#6245);
#5572=AXIS2_PLACEMENT_3D('',#7812,#6246,#6247);
#5573=AXIS2_PLACEMENT_3D('',#7813,#6248,#6249);
#5574=AXIS2_PLACEMENT_3D('',#7815,#6250,#6251);
#5575=AXIS2_PLACEMENT_3D('',#7817,#6252,#6253);
#5576=AXIS2_PLACEMENT_3D('',#7818,#6254,#6255);
#5577=AXIS2_PLACEMENT_3D('',#7819,#6256,#6257);
#5578=AXIS2_PLACEMENT_3D('',#7822,#6259,#6260);
#5579=AXIS2_PLACEMENT_3D('',#7823,#6261,#6262);
#5580=AXIS2_PLACEMENT_3D('',#7825,#6263,#6264);
#5581=AXIS2_PLACEMENT_3D('',#7828,#6266,#6267);
#5582=AXIS2_PLACEMENT_3D('',#7829,#6268,#6269);
#5583=AXIS2_PLACEMENT_3D('',#7832,#6271,#6272);
#5584=AXIS2_PLACEMENT_3D('',#7833,#6273,#6274);
#5585=AXIS2_PLACEMENT_3D('',#7834,#6275,#6276);
#5586=AXIS2_PLACEMENT_3D('',#7836,#6277,#6278);
#5587=AXIS2_PLACEMENT_3D('',#7838,#6280,#6281);
#5588=AXIS2_PLACEMENT_3D('',#7840,#6282,#6283);
#5589=AXIS2_PLACEMENT_3D('',#7841,#6284,#6285);
#5590=AXIS2_PLACEMENT_3D('',#7843,#6287,#6288);
#5591=AXIS2_PLACEMENT_3D('',#7844,#6289,#6290);
#5592=AXIS2_PLACEMENT_3D('',#7847,#6291,#6292);
#5593=AXIS2_PLACEMENT_3D('',#7848,#6293,#6294);
#5594=AXIS2_PLACEMENT_3D('',#7850,#6295,#6296);
#5595=AXIS2_PLACEMENT_3D('',#7852,#6297,#6298);
#5596=AXIS2_PLACEMENT_3D('',#7853,#6299,#6300);
#5597=AXIS2_PLACEMENT_3D('',#7854,#6301,#6302);
#5598=AXIS2_PLACEMENT_3D('',#7856,#6303,#6304);
#5599=AXIS2_PLACEMENT_3D('',#7858,#6306,#6307);
#5600=AXIS2_PLACEMENT_3D('',#7860,#6308,#6309);
#5601=AXIS2_PLACEMENT_3D('',#7862,#6310,#6311);
#5602=AXIS2_PLACEMENT_3D('',#7863,#6312,#6313);
#5603=AXIS2_PLACEMENT_3D('',#7865,#6314,#6315);
#5604=AXIS2_PLACEMENT_3D('',#7867,#6317,#6318);
#5605=AXIS2_PLACEMENT_3D('',#7869,#6319,#6320);
#5606=AXIS2_PLACEMENT_3D('',#7871,#6322,#6323);
#5607=AXIS2_PLACEMENT_3D('',#7873,#6324,#6325);
#5608=AXIS2_PLACEMENT_3D('',#7875,#6327,#6328);
#5609=AXIS2_PLACEMENT_3D('',#7876,#6329,#6330);
#5610=AXIS2_PLACEMENT_3D('',#7878,#6332,#6333);
#5611=AXIS2_PLACEMENT_3D('',#7879,#6334,#6335);
#5612=AXIS2_PLACEMENT_3D('',#7882,#6336,#6337);
#5613=AXIS2_PLACEMENT_3D('',#7883,#6338,#6339);
#5614=AXIS2_PLACEMENT_3D('',#7886,#6340,#6341);
#5615=AXIS2_PLACEMENT_3D('',#7887,#6342,#6343);
#5616=AXIS2_PLACEMENT_3D('',#7890,#6344,#6345);
#5617=AXIS2_PLACEMENT_3D('',#7891,#6346,#6347);
#5618=AXIS2_PLACEMENT_3D('',#7894,#6348,#6349);
#5619=AXIS2_PLACEMENT_3D('',#7895,#6350,#6351);
#5620=AXIS2_PLACEMENT_3D('',#7898,#6352,#6353);
#5621=AXIS2_PLACEMENT_3D('',#7899,#6354,#6355);
#5622=AXIS2_PLACEMENT_3D('',#7902,#6356,#6357);
#5623=AXIS2_PLACEMENT_3D('',#7903,#6358,#6359);
#5624=AXIS2_PLACEMENT_3D('',#7906,#6360,#6361);
#5625=AXIS2_PLACEMENT_3D('',#7907,#6362,#6363);
#5626=AXIS2_PLACEMENT_3D('',#7910,#6364,#6365);
#5627=AXIS2_PLACEMENT_3D('',#7911,#6366,#6367);
#5628=AXIS2_PLACEMENT_3D('',#7912,#6368,#6369);
#5629=AXIS2_PLACEMENT_3D('',#7938,#6370,#6371);
#5630=AXIS2_PLACEMENT_3D('',#7962,#6372,#6373);
#5631=AXIS2_PLACEMENT_3D('',#7963,#6374,#6375);
#5632=AXIS2_PLACEMENT_3D('',#7965,#6376,#6377);
#5633=AXIS2_PLACEMENT_3D('',#7990,#6378,#6379);
#5634=AXIS2_PLACEMENT_3D('',#8015,#6380,#6381);
#5635=AXIS2_PLACEMENT_3D('',#8031,#6383,#6384);
#5636=AXIS2_PLACEMENT_3D('',#8046,#6385,#6386);
#5637=AXIS2_PLACEMENT_3D('',#8071,#6387,#6388);
#5638=AXIS2_PLACEMENT_3D('',#8096,#6389,#6390);
#5639=AXIS2_PLACEMENT_3D('',#8121,#6391,#6392);
#5640=AXIS2_PLACEMENT_3D('',#8145,#6393,#6394);
#5641=AXIS2_PLACEMENT_3D('',#8146,#6395,#6396);
#5642=AXIS2_PLACEMENT_3D('',#8148,#6397,#6398);
#5643=AXIS2_PLACEMENT_3D('',#8149,#6399,#6400);
#5644=AXIS2_PLACEMENT_3D('',#8150,#6401,#6402);
#5645=AXIS2_PLACEMENT_3D('',#8174,#6403,#6404);
#5646=AXIS2_PLACEMENT_3D('',#8175,#6405,#6406);
#5647=AXIS2_PLACEMENT_3D('',#8177,#6407,#6408);
#5648=AXIS2_PLACEMENT_3D('',#8178,#6409,#6410);
#5649=AXIS2_PLACEMENT_3D('',#8179,#6411,#6412);
#5650=AXIS2_PLACEMENT_3D('',#8203,#6413,#6414);
#5651=AXIS2_PLACEMENT_3D('',#8204,#6415,#6416);
#5652=AXIS2_PLACEMENT_3D('',#8206,#6417,#6418);
#5653=AXIS2_PLACEMENT_3D('',#8207,#6419,#6420);
#5654=AXIS2_PLACEMENT_3D('',#8208,#6421,#6422);
#5655=AXIS2_PLACEMENT_3D('',#8223,#6423,#6424);
#5656=AXIS2_PLACEMENT_3D('',#8236,#6425,#6426);
#5657=AXIS2_PLACEMENT_3D('',#8238,#6427,#6428);
#5658=AXIS2_PLACEMENT_3D('',#8239,#6429,#6430);
#5659=AXIS2_PLACEMENT_3D('',#8240,#6431,#6432);
#5660=AXIS2_PLACEMENT_3D('',#8264,#6433,#6434);
#5661=AXIS2_PLACEMENT_3D('',#8265,#6435,#6436);
#5662=AXIS2_PLACEMENT_3D('',#8267,#6437,#6438);
#5663=AXIS2_PLACEMENT_3D('',#8268,#6439,#6440);
#5664=AXIS2_PLACEMENT_3D('',#8269,#6441,#6442);
#5665=AXIS2_PLACEMENT_3D('',#8293,#6443,#6444);
#5666=AXIS2_PLACEMENT_3D('',#8294,#6445,#6446);
#5667=AXIS2_PLACEMENT_3D('',#8296,#6447,#6448);
#5668=AXIS2_PLACEMENT_3D('',#8297,#6449,#6450);
#5669=AXIS2_PLACEMENT_3D('',#8298,#6451,#6452);
#5670=AXIS2_PLACEMENT_3D('',#8322,#6453,#6454);
#5671=AXIS2_PLACEMENT_3D('',#8323,#6455,#6456);
#5672=AXIS2_PLACEMENT_3D('',#8325,#6457,#6458);
#5673=AXIS2_PLACEMENT_3D('',#8328,#6460,#6461);
#5674=AXIS2_PLACEMENT_3D('',#8352,#6462,#6463);
#5675=AXIS2_PLACEMENT_3D('',#8353,#6464,#6465);
#5676=AXIS2_PLACEMENT_3D('',#8354,#6466,#6467);
#5677=AXIS2_PLACEMENT_3D('',#8355,#6468,#6469);
#5678=AXIS2_PLACEMENT_3D('',#8356,#6470,#6471);
#5679=AXIS2_PLACEMENT_3D('',#8357,#6472,#6473);
#5680=AXIS2_PLACEMENT_3D('',#8358,#6474,#6475);
#5681=AXIS2_PLACEMENT_3D('',#8359,#6476,#6477);
#5682=AXIS2_PLACEMENT_3D('',#8360,#6478,#6479);
#5683=AXIS2_PLACEMENT_3D('',#8362,#6480,#6481);
#5684=AXIS2_PLACEMENT_3D('',#8364,#6482,#6483);
#5685=AXIS2_PLACEMENT_3D('',#8365,#6484,#6485);
#5686=AXIS2_PLACEMENT_3D('',#8367,#6486,#6487);
#5687=AXIS2_PLACEMENT_3D('',#8369,#6489,#6490);
#5688=AXIS2_PLACEMENT_3D('',#8371,#6491,#6492);
#5689=AXIS2_PLACEMENT_3D('',#8372,#6493,#6494);
#5690=AXIS2_PLACEMENT_3D('',#8374,#6496,#6497);
#5691=AXIS2_PLACEMENT_3D('',#8376,#6498,#6499);
#5692=AXIS2_PLACEMENT_3D('',#8378,#6500,#6501);
#5693=AXIS2_PLACEMENT_3D('',#8379,#6502,#6503);
#5694=AXIS2_PLACEMENT_3D('',#8381,#6504,#6505);
#5695=AXIS2_PLACEMENT_3D('',#8383,#6507,#6508);
#5696=AXIS2_PLACEMENT_3D('',#8385,#6509,#6510);
#5697=AXIS2_PLACEMENT_3D('',#8386,#6511,#6512);
#5698=AXIS2_PLACEMENT_3D('',#8388,#6514,#6515);
#5699=AXIS2_PLACEMENT_3D('',#8389,#6516,#6517);
#5700=AXIS2_PLACEMENT_3D('',#8390,#6518,#6519);
#5701=AXIS2_PLACEMENT_3D('',#8391,#6520,#6521);
#5702=AXIS2_PLACEMENT_3D('',#8392,#6522,#6523);
#5703=AXIS2_PLACEMENT_3D('',#8393,#6524,#6525);
#5704=AXIS2_PLACEMENT_3D('',#8394,#6526,#6527);
#5705=AXIS2_PLACEMENT_3D('',#8399,#6529,#6530);
#5706=AXIS2_PLACEMENT_3D('',#8402,#6532,#6533);
#5707=AXIS2_PLACEMENT_3D('',#8403,#6534,#6535);
#5708=AXIS2_PLACEMENT_3D('',#8408,#6537,#6538);
#5709=AXIS2_PLACEMENT_3D('',#8411,#6540,#6541);
#5710=AXIS2_PLACEMENT_3D('',#8412,#6542,#6543);
#5711=AXIS2_PLACEMENT_3D('',#8418,#6547,#6548);
#5712=AXIS2_PLACEMENT_3D('',#8425,#6552,#6553);
#5713=AXIS2_PLACEMENT_3D('',#8426,#6554,#6555);
#5714=AXIS2_PLACEMENT_3D('',#8430,#6558,#6559);
#5715=AXIS2_PLACEMENT_3D('',#8433,#6561,#6562);
#5716=AXIS2_PLACEMENT_3D('',#8434,#6563,#6564);
#5717=AXIS2_PLACEMENT_3D('',#8438,#6567,#6568);
#5718=AXIS2_PLACEMENT_3D('',#8443,#6571,#6572);
#5719=AXIS2_PLACEMENT_3D('',#8444,#6573,#6574);
#5720=AXIS2_PLACEMENT_3D('',#8446,#6575,#6576);
#5721=AXIS2_PLACEMENT_3D('',#8449,#6578,#6579);
#5722=AXIS2_PLACEMENT_3D('',#8450,#6580,#6581);
#5723=AXIS2_PLACEMENT_3D('',#8455,#6583,#6584);
#5724=AXIS2_PLACEMENT_3D('',#8458,#6586,#6587);
#5725=AXIS2_PLACEMENT_3D('',#8459,#6588,#6589);
#5726=AXIS2_PLACEMENT_3D('',#8460,#6590,#6591);
#5727=AXIS2_PLACEMENT_3D('',#8461,#6592,#6593);
#5728=AXIS2_PLACEMENT_3D('',#8467,#6597,#6598);
#5729=AXIS2_PLACEMENT_3D('',#8471,#6601,#6602);
#5730=AXIS2_PLACEMENT_3D('',#8475,#6605,#6606);
#5731=AXIS2_PLACEMENT_3D('',#8477,#6607,#6608);
#5732=AXIS2_PLACEMENT_3D('',#8480,#6610,#6611);
#5733=AXIS2_PLACEMENT_3D('',#8481,#6612,#6613);
#5734=AXIS2_PLACEMENT_3D('',#8483,#6615,#6616);
#5735=AXIS2_PLACEMENT_3D('',#8485,#6618,#6619);
#5736=AXIS2_PLACEMENT_3D('',#8487,#6621,#6622);
#5737=AXIS2_PLACEMENT_3D('',#8496,#6627,#6628);
#5738=AXIS2_PLACEMENT_3D('',#8502,#6632,#6633);
#5739=AXIS2_PLACEMENT_3D('',#8508,#6637,#6638);
#5740=AXIS2_PLACEMENT_3D('',#8511,#6641,#6642);
#5741=AXIS2_PLACEMENT_3D('',#8512,#6643,#6644);
#5742=AXIS2_PLACEMENT_3D('',#8513,#6645,#6646);
#5743=AXIS2_PLACEMENT_3D('',#8514,#6647,#6648);
#5744=AXIS2_PLACEMENT_3D('',#8516,#6649,#6650);
#5745=AXIS2_PLACEMENT_3D('',#8519,#6652,#6653);
#5746=AXIS2_PLACEMENT_3D('',#8520,#6654,#6655);
#5747=AXIS2_PLACEMENT_3D('',#8522,#6656,#6657);
#5748=AXIS2_PLACEMENT_3D('',#8525,#6659,#6660);
#5749=AXIS2_PLACEMENT_3D('',#8526,#6661,#6662);
#5750=AXIS2_PLACEMENT_3D('',#8535,#6667,#6668);
#5751=AXIS2_PLACEMENT_3D('',#8541,#6672,#6673);
#5752=AXIS2_PLACEMENT_3D('',#8547,#6677,#6678);
#5753=AXIS2_PLACEMENT_3D('',#8553,#6682,#6683);
#5754=AXIS2_PLACEMENT_3D('',#8559,#6687,#6688);
#5755=AXIS2_PLACEMENT_3D('',#8561,#6690,#6691);
#5756=AXIS2_PLACEMENT_3D('',#8563,#6693,#6694);
#5757=AXIS2_PLACEMENT_3D('',#8564,#6695,#6696);
#5758=AXIS2_PLACEMENT_3D('',#8565,#6697,#6698);
#5759=AXIS2_PLACEMENT_3D('',#8570,#6700,#6701);
#5760=AXIS2_PLACEMENT_3D('',#8573,#6703,#6704);
#5761=AXIS2_PLACEMENT_3D('',#8574,#6705,#6706);
#5762=AXIS2_PLACEMENT_3D('',#8579,#6708,#6709);
#5763=AXIS2_PLACEMENT_3D('',#8582,#6711,#6712);
#5764=AXIS2_PLACEMENT_3D('',#8583,#6713,#6714);
#5765=AXIS2_PLACEMENT_3D('',#8589,#6718,#6719);
#5766=AXIS2_PLACEMENT_3D('',#8596,#6723,#6724);
#5767=AXIS2_PLACEMENT_3D('',#8597,#6725,#6726);
#5768=AXIS2_PLACEMENT_3D('',#8601,#6729,#6730);
#5769=AXIS2_PLACEMENT_3D('',#8604,#6732,#6733);
#5770=AXIS2_PLACEMENT_3D('',#8605,#6734,#6735);
#5771=AXIS2_PLACEMENT_3D('',#8609,#6738,#6739);
#5772=AXIS2_PLACEMENT_3D('',#8614,#6742,#6743);
#5773=AXIS2_PLACEMENT_3D('',#8615,#6744,#6745);
#5774=AXIS2_PLACEMENT_3D('',#8617,#6746,#6747);
#5775=AXIS2_PLACEMENT_3D('',#8620,#6749,#6750);
#5776=AXIS2_PLACEMENT_3D('',#8621,#6751,#6752);
#5777=AXIS2_PLACEMENT_3D('',#8626,#6754,#6755);
#5778=AXIS2_PLACEMENT_3D('',#8629,#6757,#6758);
#5779=AXIS2_PLACEMENT_3D('',#8630,#6759,#6760);
#5780=AXIS2_PLACEMENT_3D('',#8631,#6761,#6762);
#5781=AXIS2_PLACEMENT_3D('',#8632,#6763,#6764);
#5782=AXIS2_PLACEMENT_3D('',#8638,#6768,#6769);
#5783=AXIS2_PLACEMENT_3D('',#8642,#6772,#6773);
#5784=AXIS2_PLACEMENT_3D('',#8646,#6776,#6777);
#5785=AXIS2_PLACEMENT_3D('',#8648,#6778,#6779);
#5786=AXIS2_PLACEMENT_3D('',#8651,#6781,#6782);
#5787=AXIS2_PLACEMENT_3D('',#8652,#6783,#6784);
#5788=AXIS2_PLACEMENT_3D('',#8654,#6786,#6787);
#5789=AXIS2_PLACEMENT_3D('',#8656,#6789,#6790);
#5790=AXIS2_PLACEMENT_3D('',#8658,#6792,#6793);
#5791=AXIS2_PLACEMENT_3D('',#8667,#6798,#6799);
#5792=AXIS2_PLACEMENT_3D('',#8673,#6803,#6804);
#5793=AXIS2_PLACEMENT_3D('',#8679,#6808,#6809);
#5794=AXIS2_PLACEMENT_3D('',#8682,#6812,#6813);
#5795=AXIS2_PLACEMENT_3D('',#8683,#6814,#6815);
#5796=AXIS2_PLACEMENT_3D('',#8684,#6816,#6817);
#5797=AXIS2_PLACEMENT_3D('',#8685,#6818,#6819);
#5798=AXIS2_PLACEMENT_3D('',#8687,#6820,#6821);
#5799=AXIS2_PLACEMENT_3D('',#8690,#6823,#6824);
#5800=AXIS2_PLACEMENT_3D('',#8691,#6825,#6826);
#5801=AXIS2_PLACEMENT_3D('',#8693,#6827,#6828);
#5802=AXIS2_PLACEMENT_3D('',#8696,#6830,#6831);
#5803=AXIS2_PLACEMENT_3D('',#8697,#6832,#6833);
#5804=AXIS2_PLACEMENT_3D('',#8706,#6838,#6839);
#5805=AXIS2_PLACEMENT_3D('',#8712,#6843,#6844);
#5806=AXIS2_PLACEMENT_3D('',#8718,#6848,#6849);
#5807=AXIS2_PLACEMENT_3D('',#8724,#6853,#6854);
#5808=AXIS2_PLACEMENT_3D('',#8730,#6858,#6859);
#5809=AXIS2_PLACEMENT_3D('',#8732,#6861,#6862);
#5810=AXIS2_PLACEMENT_3D('',#8734,#6864,#6865);
#5811=AXIS2_PLACEMENT_3D('',#8735,#6866,#6867);
#5812=AXIS2_PLACEMENT_3D('',#8736,#6868,#6869);
#5813=AXIS2_PLACEMENT_3D('',#8745,#6874,#6875);
#5814=AXIS2_PLACEMENT_3D('',#8751,#6879,#6880);
#5815=AXIS2_PLACEMENT_3D('',#8757,#6884,#6885);
#5816=AXIS2_PLACEMENT_3D('',#8763,#6889,#6890);
#5817=AXIS2_PLACEMENT_3D('',#8769,#6894,#6895);
#5818=AXIS2_PLACEMENT_3D('',#8775,#6899,#6900);
#5819=AXIS2_PLACEMENT_3D('',#8781,#6904,#6905);
#5820=AXIS2_PLACEMENT_3D('',#8787,#6909,#6910);
#5821=AXIS2_PLACEMENT_3D('',#8793,#6914,#6915);
#5822=AXIS2_PLACEMENT_3D('',#8802,#6920,#6921);
#5823=AXIS2_PLACEMENT_3D('',#8808,#6925,#6926);
#5824=AXIS2_PLACEMENT_3D('',#8814,#6930,#6931);
#5825=AXIS2_PLACEMENT_3D('',#8820,#6935,#6936);
#5826=AXIS2_PLACEMENT_3D('',#8826,#6940,#6941);
#5827=AXIS2_PLACEMENT_3D('',#8832,#6945,#6946);
#5828=AXIS2_PLACEMENT_3D('',#8838,#6950,#6951);
#5829=AXIS2_PLACEMENT_3D('',#8844,#6955,#6956);
#5830=AXIS2_PLACEMENT_3D('',#8850,#6960,#6961);
#5831=AXIS2_PLACEMENT_3D('',#8859,#6966,#6967);
#5832=AXIS2_PLACEMENT_3D('',#8865,#6971,#6972);
#5833=AXIS2_PLACEMENT_3D('',#8871,#6976,#6977);
#5834=AXIS2_PLACEMENT_3D('',#8877,#6981,#6982);
#5835=AXIS2_PLACEMENT_3D('',#8883,#6986,#6987);
#5836=AXIS2_PLACEMENT_3D('',#8889,#6991,#6992);
#5837=AXIS2_PLACEMENT_3D('',#8895,#6996,#6997);
#5838=AXIS2_PLACEMENT_3D('',#8901,#7001,#7002);
#5839=AXIS2_PLACEMENT_3D('',#8907,#7006,#7007);
#5840=AXIS2_PLACEMENT_3D('',#8916,#7012,#7013);
#5841=AXIS2_PLACEMENT_3D('',#8922,#7017,#7018);
#5842=AXIS2_PLACEMENT_3D('',#8928,#7022,#7023);
#5843=AXIS2_PLACEMENT_3D('',#8934,#7027,#7028);
#5844=AXIS2_PLACEMENT_3D('',#8940,#7032,#7033);
#5845=AXIS2_PLACEMENT_3D('',#8946,#7037,#7038);
#5846=AXIS2_PLACEMENT_3D('',#8952,#7042,#7043);
#5847=AXIS2_PLACEMENT_3D('',#8958,#7047,#7048);
#5848=AXIS2_PLACEMENT_3D('',#8964,#7052,#7053);
#5849=AXIS2_PLACEMENT_3D('',#8966,#7054,#7055);
#5850=AXIS2_PLACEMENT_3D('',#8969,#7057,#7058);
#5851=AXIS2_PLACEMENT_3D('',#8970,#7059,#7060);
#5852=AXIS2_PLACEMENT_3D('',#8976,#7064,#7065);
#5853=AXIS2_PLACEMENT_3D('',#8982,#7069,#7070);
#5854=AXIS2_PLACEMENT_3D('',#8985,#7073,#7074);
#5855=AXIS2_PLACEMENT_3D('',#8991,#7078,#7079);
#5856=AXIS2_PLACEMENT_3D('',#8994,#7082,#7083);
#5857=AXIS2_PLACEMENT_3D('',#9000,#7087,#7088);
#5858=AXIS2_PLACEMENT_3D('',#9003,#7091,#7092);
#5859=AXIS2_PLACEMENT_3D('',#9006,#7095,#7096);
#5860=AXIS2_PLACEMENT_3D('',#9007,#7097,#7098);
#5861=AXIS2_PLACEMENT_3D('',#9008,#7099,#7100);
#5862=AXIS2_PLACEMENT_3D('',#9009,#7101,#7102);
#5863=AXIS2_PLACEMENT_3D('',#9020,#7107,#7108);
#5864=AXIS2_PLACEMENT_3D('',#9022,#7110,#7111);
#5865=AXIS2_PLACEMENT_3D('',#9024,#7112,#7113);
#5866=AXIS2_PLACEMENT_3D('',#9027,#7115,#7116);
#5867=AXIS2_PLACEMENT_3D('',#9029,#7117,#7118);
#5868=AXIS2_PLACEMENT_3D('',#9031,#7119,#7120);
#5869=AXIS2_PLACEMENT_3D('',#9032,#7121,#7122);
#5870=AXIS2_PLACEMENT_3D('',#9033,#7123,#7124);
#5871=AXIS2_PLACEMENT_3D('',#9037,#7127,#7128);
#5872=AXIS2_PLACEMENT_3D('',#9041,#7131,#7132);
#5873=AXIS2_PLACEMENT_3D('',#9047,#7136,#7137);
#5874=AXIS2_PLACEMENT_3D('',#9053,#7141,#7142);
#5875=AXIS2_PLACEMENT_3D('',#9057,#7145,#7146);
#5876=AXIS2_PLACEMENT_3D('',#9061,#7149,#7150);
#5877=AXIS2_PLACEMENT_3D('',#9063,#7152,#7153);
#5878=AXIS2_PLACEMENT_3D('',#9064,#7154,#7155);
#5879=AXIS2_PLACEMENT_3D('',#9065,#7156,#7157);
#5880=AXIS2_PLACEMENT_3D('',#9067,#7158,#7159);
#5881=AXIS2_PLACEMENT_3D('',#9070,#7161,#7162);
#5882=AXIS2_PLACEMENT_3D('',#9071,#7163,#7164);
#5883=AXIS2_PLACEMENT_3D('',#9074,#7166,#7167);
#5884=AXIS2_PLACEMENT_3D('',#9075,#7168,#7169);
#5885=AXIS2_PLACEMENT_3D('',#9077,#7170,#7171);
#5886=AXIS2_PLACEMENT_3D('',#9078,#7172,#7173);
#5887=AXIS2_PLACEMENT_3D('',#9081,#7175,#7176);
#5888=AXIS2_PLACEMENT_3D('',#9082,#7177,#7178);
#5889=AXIS2_PLACEMENT_3D('',#9083,#7179,#7180);
#5890=AXIS2_PLACEMENT_3D('',#9084,#7181,#7182);
#5891=AXIS2_PLACEMENT_3D('',#9093,#7187,#7188);
#5892=AXIS2_PLACEMENT_3D('',#9099,#7192,#7193);
#5893=AXIS2_PLACEMENT_3D('',#9105,#7197,#7198);
#5894=AXIS2_PLACEMENT_3D('',#9111,#7202,#7203);
#5895=AXIS2_PLACEMENT_3D('',#9117,#7207,#7208);
#5896=AXIS2_PLACEMENT_3D('',#9120,#7211,#7212);
#5897=AXIS2_PLACEMENT_3D('',#9121,#7213,#7214);
#5898=AXIS2_PLACEMENT_3D('',#9122,#7215,#7216);
#5899=AXIS2_PLACEMENT_3D('',#9124,#7217,#7218);
#5900=AXIS2_PLACEMENT_3D('',#9125,#7219,#7220);
#5901=AXIS2_PLACEMENT_3D('',#9127,#7221,#7222);
#5902=AXIS2_PLACEMENT_3D('',#9128,#7223,#7224);
#5903=AXIS2_PLACEMENT_3D('',#9130,#7225,#7226);
#5904=AXIS2_PLACEMENT_3D('',#9132,#7228,#7229);
#5905=AXIS2_PLACEMENT_3D('',#9134,#7230,#7231);
#5906=AXIS2_PLACEMENT_3D('',#9136,#7233,#7234);
#5907=AXIS2_PLACEMENT_3D('',#9138,#7235,#7236);
#5908=AXIS2_PLACEMENT_3D('',#9140,#7238,#7239);
#5909=AXIS2_PLACEMENT_3D('',#9142,#7240,#7241);
#5910=AXIS2_PLACEMENT_3D('',#9143,#7242,#7243);
#5911=AXIS2_PLACEMENT_3D('',#9145,#7244,#7245);
#5912=AXIS2_PLACEMENT_3D('',#9147,#7247,#7248);
#5913=AXIS2_PLACEMENT_3D('',#9149,#7250,#7251);
#5914=AXIS2_PLACEMENT_3D('',#9150,#7252,#7253);
#5915=AXIS2_PLACEMENT_3D('',#9152,#7254,#7255);
#5916=AXIS2_PLACEMENT_3D('',#9155,#7257,#7258);
#5917=AXIS2_PLACEMENT_3D('',#9156,#7259,#7260);
#5918=AXIS2_PLACEMENT_3D('',#9158,#7261,#7262);
#5919=AXIS2_PLACEMENT_3D('',#9160,#7264,#7265);
#5920=AXIS2_PLACEMENT_3D('',#9161,#7266,#7267);
#5921=AXIS2_PLACEMENT_3D('',#9163,#7268,#7269);
#5922=AXIS2_PLACEMENT_3D('',#9189,#7271,#7272);
#5923=AXIS2_PLACEMENT_3D('',#9195,#7276,#7277);
#5924=AXIS2_PLACEMENT_3D('',#9199,#7280,#7281);
#5925=AXIS2_PLACEMENT_3D('',#9203,#7284,#7285);
#5926=AXIS2_PLACEMENT_3D('',#9207,#7288,#7289);
#5927=AXIS2_PLACEMENT_3D('',#9211,#7292,#7293);
#5928=AXIS2_PLACEMENT_3D('',#9213,#7295,#7296);
#5929=AXIS2_PLACEMENT_3D('',#9214,#7297,#7298);
#5930=AXIS2_PLACEMENT_3D('',#9215,#7299,#7300);
#5931=AXIS2_PLACEMENT_3D('',#9216,#7301,#7302);
#5932=AXIS2_PLACEMENT_3D('',#9228,#7304,#7305);
#5933=AXIS2_PLACEMENT_3D('',#9244,#7306,#7307);
#5934=AXIS2_PLACEMENT_3D('',#9246,#7308,#7309);
#5935=AXIS2_PLACEMENT_3D('',#9272,#7311,#7312);
#5936=AXIS2_PLACEMENT_3D('',#9275,#7315,#7316);
#5937=AXIS2_PLACEMENT_3D('',#9277,#7318,#7319);
#5938=AXIS2_PLACEMENT_3D('',#9279,#7321,#7322);
#5939=AXIS2_PLACEMENT_3D('',#9281,#7323,#7324);
#5940=AXIS2_PLACEMENT_3D('',#9284,#7326,#7327);
#5941=AXIS2_PLACEMENT_3D('',#9285,#7328,#7329);
#5942=AXIS2_PLACEMENT_3D('',#9287,#7331,#7332);
#5943=AXIS2_PLACEMENT_3D('',#9289,#7334,#7335);
#5944=AXIS2_PLACEMENT_3D('',#9290,#7336,#7337);
#5945=AXIS2_PLACEMENT_3D('',#9291,#7338,#7339);
#5946=AXIS2_PLACEMENT_3D('',#9292,#7340,#7341);
#5947=AXIS2_PLACEMENT_3D('',#9293,#7342,#7343);
#5948=AXIS2_PLACEMENT_3D('',#9294,#7344,#7345);
#5949=AXIS2_PLACEMENT_3D('',#9296,#7346,#7347);
#5950=AXIS2_PLACEMENT_3D('',#9299,#7349,#7350);
#5951=AXIS2_PLACEMENT_3D('',#9300,#7351,#7352);
#5952=AXIS2_PLACEMENT_3D('',#9302,#7353,#7354);
#5953=AXIS2_PLACEMENT_3D('',#9305,#7356,#7357);
#5954=AXIS2_PLACEMENT_3D('',#9306,#7358,#7359);
#5955=AXIS2_PLACEMENT_3D('',#9308,#7360,#7361);
#5956=AXIS2_PLACEMENT_3D('',#9311,#7363,#7364);
#5957=AXIS2_PLACEMENT_3D('',#9312,#7365,#7366);
#5958=AXIS2_PLACEMENT_3D('',#9314,#7367,#7368);
#5959=AXIS2_PLACEMENT_3D('',#9317,#7370,#7371);
#5960=AXIS2_PLACEMENT_3D('',#9318,#7372,#7373);
#5961=AXIS2_PLACEMENT_3D('',#9320,#7374,#7375);
#5962=AXIS2_PLACEMENT_3D('',#9323,#7377,#7378);
#5963=AXIS2_PLACEMENT_3D('',#9324,#7379,#7380);
#5964=AXIS2_PLACEMENT_3D('',#9326,#7381,#7382);
#5965=AXIS2_PLACEMENT_3D('',#9327,#7383,#7384);
#5966=AXIS2_PLACEMENT_3D('',#9330,#7386,#7387);
#5967=AXIS2_PLACEMENT_3D('',#9331,#7388,#7389);
#5968=AXIS2_PLACEMENT_3D('',#9333,#7390,#7391);
#5969=AXIS2_PLACEMENT_3D('',#9336,#7393,#7394);
#5970=AXIS2_PLACEMENT_3D('',#9337,#7395,#7396);
#5971=AXIS2_PLACEMENT_3D('',#9338,#7397,#7398);
#5972=AXIS2_PLACEMENT_3D('',#9339,#7399,#7400);
#5973=AXIS2_PLACEMENT_3D('',#9340,#7401,#7402);
#5974=AXIS2_PLACEMENT_3D('',#9342,#7403,#7404);
#5975=AXIS2_PLACEMENT_3D('',#9345,#7406,#7407);
#5976=AXIS2_PLACEMENT_3D('',#9346,#7408,#7409);
#5977=AXIS2_PLACEMENT_3D('',#9348,#7410,#7411);
#5978=AXIS2_PLACEMENT_3D('',#9351,#7413,#7414);
#5979=AXIS2_PLACEMENT_3D('',#9352,#7415,#7416);
#5980=AXIS2_PLACEMENT_3D('',#9354,#7417,#7418);
#5981=AXIS2_PLACEMENT_3D('',#9357,#7420,#7421);
#5982=AXIS2_PLACEMENT_3D('',#9358,#7422,#7423);
#5983=AXIS2_PLACEMENT_3D('',#9360,#7424,#7425);
#5984=AXIS2_PLACEMENT_3D('',#9363,#7427,#7428);
#5985=AXIS2_PLACEMENT_3D('',#9364,#7429,#7430);
#5986=AXIS2_PLACEMENT_3D('',#9366,#7431,#7432);
#5987=AXIS2_PLACEMENT_3D('',#9369,#7434,#7435);
#5988=AXIS2_PLACEMENT_3D('',#9370,#7436,#7437);
#5989=AXIS2_PLACEMENT_3D('',#9372,#7438,#7439);
#5990=AXIS2_PLACEMENT_3D('',#9373,#7440,#7441);
#5991=AXIS2_PLACEMENT_3D('',#9375,#7442,#7443);
#5992=AXIS2_PLACEMENT_3D('',#9377,#7445,#7446);
#5993=AXIS2_PLACEMENT_3D('',#9379,#7447,#7448);
#5994=AXIS2_PLACEMENT_3D('',#9382,#7450,#7451);
#5995=AXIS2_PLACEMENT_3D('',#9383,#7452,#7453);
#5996=AXIS2_PLACEMENT_3D('',#9384,#7454,#7455);
#5997=AXIS2_PLACEMENT_3D('',#9385,#7456,#7457);
#5998=AXIS2_PLACEMENT_3D('',#9386,#7458,#7459);
#5999=AXIS2_PLACEMENT_3D('',#9388,#7460,#7461);
#6000=AXIS2_PLACEMENT_3D('',#9391,#7463,#7464);
#6001=AXIS2_PLACEMENT_3D('',#9392,#7465,#7466);
#6002=AXIS2_PLACEMENT_3D('',#9394,#7467,#7468);
#6003=AXIS2_PLACEMENT_3D('',#9397,#7470,#7471);
#6004=AXIS2_PLACEMENT_3D('',#9398,#7472,#7473);
#6005=AXIS2_PLACEMENT_3D('',#9399,#7474,#7475);
#6006=AXIS2_PLACEMENT_3D('',#9400,#7476,#7477);
#6007=AXIS2_PLACEMENT_3D('',#9401,#7478,#7479);
#6008=AXIS2_PLACEMENT_3D('',#9403,#7480,#7481);
#6009=AXIS2_PLACEMENT_3D('',#9406,#7483,#7484);
#6010=AXIS2_PLACEMENT_3D('',#9407,#7485,#7486);
#6011=AXIS2_PLACEMENT_3D('',#9409,#7487,#7488);
#6012=AXIS2_PLACEMENT_3D('',#9412,#7490,#7491);
#6013=AXIS2_PLACEMENT_3D('',#9413,#7492,#7493);
#6014=AXIS2_PLACEMENT_3D('',#9415,#7494,#7495);
#6015=AXIS2_PLACEMENT_3D('',#9418,#7497,#7498);
#6016=AXIS2_PLACEMENT_3D('',#9419,#7499,#7500);
#6017=AXIS2_PLACEMENT_3D('',#9421,#7501,#7502);
#6018=AXIS2_PLACEMENT_3D('',#9424,#7504,#7505);
#6019=AXIS2_PLACEMENT_3D('',#9425,#7506,#7507);
#6020=AXIS2_PLACEMENT_3D('',#9427,#7508,#7509);
#6021=AXIS2_PLACEMENT_3D('',#9430,#7511,#7512);
#6022=AXIS2_PLACEMENT_3D('',#9431,#7513,#7514);
#6023=AXIS2_PLACEMENT_3D('',#9433,#7515,#7516);
#6024=AXIS2_PLACEMENT_3D('',#9436,#7518,#7519);
#6025=AXIS2_PLACEMENT_3D('',#9437,#7520,#7521);
#6026=AXIS2_PLACEMENT_3D('',#9438,#7522,#7523);
#6027=AXIS2_PLACEMENT_3D('',#9439,#7524,#7525);
#6028=AXIS2_PLACEMENT_3D('',#9440,#7526,#7527);
#6029=AXIS2_PLACEMENT_3D('',#9442,#7528,#7529);
#6030=AXIS2_PLACEMENT_3D('',#9443,#7530,#7531);
#6031=AXIS2_PLACEMENT_3D('',#9445,#7532,#7533);
#6032=AXIS2_PLACEMENT_3D('',#9447,#7535,#7536);
#6033=AXIS2_PLACEMENT_3D('',#9449,#7537,#7538);
#6034=AXIS2_PLACEMENT_3D('',#9451,#7540,#7541);
#6035=AXIS2_PLACEMENT_3D('',#9453,#7542,#7543);
#6036=AXIS2_PLACEMENT_3D('',#9455,#7545,#7546);
#6037=AXIS2_PLACEMENT_3D('',#9457,#7547,#7548);
#6038=AXIS2_PLACEMENT_3D('',#9458,#7549,#7550);
#6039=AXIS2_PLACEMENT_3D('',#9460,#7551,#7552);
#6040=AXIS2_PLACEMENT_3D('',#9462,#7554,#7555);
#6041=AXIS2_PLACEMENT_3D('',#9464,#7556,#7557);
#6042=AXIS2_PLACEMENT_3D('',#9466,#7559,#7560);
#6043=AXIS2_PLACEMENT_3D('',#9468,#7561,#7562);
#6044=AXIS2_PLACEMENT_3D('',#9470,#7564,#7565);
#6045=AXIS2_PLACEMENT_3D('',#9471,#7566,#7567);
#6046=AXIS2_PLACEMENT_3D('',#9480,#7572,#7573);
#6047=AXIS2_PLACEMENT_3D('',#9486,#7577,#7578);
#6048=AXIS2_PLACEMENT_3D('',#9492,#7582,#7583);
#6049=AXIS2_PLACEMENT_3D('',#9498,#7587,#7588);
#6050=AXIS2_PLACEMENT_3D('',#9504,#7592,#7593);
#6051=AXIS2_PLACEMENT_3D('',#9507,#7596,#7597);
#6052=AXIS2_PLACEMENT_3D('',#9508,#7598,#7599);
#6053=AXIS2_PLACEMENT_3D('',#9509,#7600,#7601);
#6054=AXIS2_PLACEMENT_3D('',#9510,#7602,#7603);
#6055=AXIS2_PLACEMENT_3D('',#9511,#7604,#7605);
#6056=AXIS2_PLACEMENT_3D('',#9512,#7606,#7607);
#6057=AXIS2_PLACEMENT_3D('',#9513,#7608,#7609);
#6058=AXIS2_PLACEMENT_3D('',#9514,#7610,#7611);
#6059=AXIS2_PLACEMENT_3D('',#9515,#7612,#7613);
#6060=AXIS2_PLACEMENT_3D('',#9516,#7614,#7615);
#6061=AXIS2_PLACEMENT_3D('',#9517,#7616,#7617);
#6062=AXIS2_PLACEMENT_3D('',#9518,#7618,#7619);
#6063=AXIS2_PLACEMENT_3D('',#9519,#7620,#7621);
#6064=AXIS2_PLACEMENT_3D('',#9520,#7622,#7623);
#6065=AXIS2_PLACEMENT_3D('',#9521,#7624,#7625);
#6066=AXIS2_PLACEMENT_3D('',#9522,#7626,#7627);
#6067=AXIS2_PLACEMENT_3D('',#9523,#7628,#7629);
#6068=AXIS2_PLACEMENT_3D('',#9524,#7630,#7631);
#6069=AXIS2_PLACEMENT_3D('',#9525,#7632,#7633);
#6070=AXIS2_PLACEMENT_3D('',#9526,#7634,#7635);
#6071=AXIS2_PLACEMENT_3D('',#9527,#7636,#7637);
#6072=AXIS2_PLACEMENT_3D('',#9528,#7638,#7639);
#6073=AXIS2_PLACEMENT_3D('',#9529,#7640,#7641);
#6074=AXIS2_PLACEMENT_3D('',#9530,#7642,#7643);
#6075=AXIS2_PLACEMENT_3D('',#9531,#7644,#7645);
#6076=AXIS2_PLACEMENT_3D('',#9532,#7646,#7647);
#6077=AXIS2_PLACEMENT_3D('',#9533,#7648,#7649);
#6078=AXIS2_PLACEMENT_3D('',#9534,#7650,#7651);
#6079=AXIS2_PLACEMENT_3D('',#9535,#7652,#7653);
#6080=AXIS2_PLACEMENT_3D('',#9536,#7654,#7655);
#6081=AXIS2_PLACEMENT_3D('',#9537,#7656,#7657);
#6082=AXIS2_PLACEMENT_3D('',#9538,#7658,#7659);
#6083=AXIS2_PLACEMENT_3D('',#9539,#7660,#7661);
#6084=AXIS2_PLACEMENT_3D('',#9540,#7662,#7663);
#6085=AXIS2_PLACEMENT_3D('',#9541,#7664,#7665);
#6086=AXIS2_PLACEMENT_3D('',#9542,#7666,#7667);
#6087=AXIS2_PLACEMENT_3D('',#9543,#7668,#7669);
#6088=AXIS2_PLACEMENT_3D('',#9544,#7670,#7671);
#6089=AXIS2_PLACEMENT_3D('',#9545,#7672,#7673);
#6090=AXIS2_PLACEMENT_3D('',#9546,#7674,#7675);
#6091=AXIS2_PLACEMENT_3D('',#9547,#7676,#7677);
#6092=AXIS2_PLACEMENT_3D('',#9548,#7678,#7679);
#6093=AXIS2_PLACEMENT_3D('',#9549,#7680,#7681);
#6094=AXIS2_PLACEMENT_3D('',#9550,#7682,#7683);
#6095=AXIS2_PLACEMENT_3D('',#9551,#7684,#7685);
#6096=AXIS2_PLACEMENT_3D('',#9552,#7686,#7687);
#6097=AXIS2_PLACEMENT_3D('',#9553,#7688,#7689);
#6098=AXIS2_PLACEMENT_3D('',#9554,#7690,#7691);
#6099=AXIS2_PLACEMENT_3D('',#9555,#7692,#7693);
#6100=AXIS2_PLACEMENT_3D('',#9556,#7694,#7695);
#6101=AXIS2_PLACEMENT_3D('',#9557,#7696,#7697);
#6102=AXIS2_PLACEMENT_3D('',#9558,#7698,#7699);
#6103=AXIS2_PLACEMENT_3D('',#9559,#7700,#7701);
#6104=AXIS2_PLACEMENT_3D('',#9560,#7702,#7703);
#6105=AXIS2_PLACEMENT_3D('',#9561,#7704,#7705);
#6106=AXIS2_PLACEMENT_3D('',#9562,#7706,#7707);
#6107=DIRECTION('axis',(0.,0.,1.));
#6108=DIRECTION('refdir',(1.,0.,0.));
#6109=DIRECTION('axis',(0.,0.,1.));
#6110=DIRECTION('refdir',(1.,0.,0.));
#6111=DIRECTION('axis',(0.,0.,1.));
#6112=DIRECTION('refdir',(1.,0.,0.));
#6113=DIRECTION('center_axis',(0.,1.,0.));
#6114=DIRECTION('ref_axis',(1.,0.,0.));
#6115=DIRECTION('center_axis',(0.,1.,0.));
#6116=DIRECTION('ref_axis',(1.,0.,0.));
#6117=DIRECTION('',(0.,1.,0.));
#6118=DIRECTION('center_axis',(0.,-1.,0.));
#6119=DIRECTION('ref_axis',(1.,0.,0.));
#6120=DIRECTION('center_axis',(0.,1.,0.));
#6121=DIRECTION('ref_axis',(1.,0.,0.));
#6122=DIRECTION('center_axis',(0.,1.,0.));
#6123=DIRECTION('ref_axis',(1.,0.,0.));
#6124=DIRECTION('center_axis',(0.,1.,0.));
#6125=DIRECTION('ref_axis',(1.,0.,0.));
#6126=DIRECTION('',(0.,1.,0.));
#6127=DIRECTION('center_axis',(0.,1.,0.));
#6128=DIRECTION('ref_axis',(1.,0.,0.));
#6129=DIRECTION('center_axis',(0.,1.,0.));
#6130=DIRECTION('ref_axis',(1.,0.,0.));
#6131=DIRECTION('center_axis',(0.,1.,0.));
#6132=DIRECTION('ref_axis',(1.,0.,0.));
#6133=DIRECTION('center_axis',(0.,1.,0.));
#6134=DIRECTION('ref_axis',(1.,0.,0.));
#6135=DIRECTION('center_axis',(0.,1.,0.));
#6136=DIRECTION('ref_axis',(1.,0.,0.));
#6137=DIRECTION('center_axis',(0.,1.,0.));
#6138=DIRECTION('ref_axis',(1.,0.,0.));
#6139=DIRECTION('center_axis',(0.,1.,0.));
#6140=DIRECTION('ref_axis',(1.,0.,0.));
#6141=DIRECTION('center_axis',(0.,-1.,0.));
#6142=DIRECTION('ref_axis',(1.,0.,0.));
#6143=DIRECTION('center_axis',(0.,1.,0.));
#6144=DIRECTION('ref_axis',(1.,0.,0.));
#6145=DIRECTION('',(0.,-1.,0.));
#6146=DIRECTION('center_axis',(0.,1.,0.));
#6147=DIRECTION('ref_axis',(1.,0.,0.));
#6148=DIRECTION('',(0.,-1.,0.));
#6149=DIRECTION('center_axis',(0.,1.,0.));
#6150=DIRECTION('ref_axis',(1.,0.,0.));
#6151=DIRECTION('center_axis',(0.,1.,0.));
#6152=DIRECTION('ref_axis',(1.,0.,0.));
#6153=DIRECTION('center_axis',(0.,1.,0.));
#6154=DIRECTION('ref_axis',(1.,0.,0.));
#6155=DIRECTION('',(0.,-1.,0.));
#6156=DIRECTION('center_axis',(0.,1.,0.));
#6157=DIRECTION('ref_axis',(1.,0.,0.));
#6158=DIRECTION('center_axis',(0.,1.,0.));
#6159=DIRECTION('ref_axis',(1.,0.,0.));
#6160=DIRECTION('axis',(0.,0.,1.));
#6161=DIRECTION('refdir',(1.,0.,0.));
#6162=DIRECTION('center_axis',(0.,1.,0.));
#6163=DIRECTION('ref_axis',(1.,0.,0.));
#6164=DIRECTION('center_axis',(0.,-1.,0.));
#6165=DIRECTION('ref_axis',(1.,0.,0.));
#6166=DIRECTION('',(0.,-1.,0.));
#6167=DIRECTION('center_axis',(0.,-1.,0.));
#6168=DIRECTION('ref_axis',(1.,0.,0.));
#6169=DIRECTION('center_axis',(0.,1.,0.));
#6170=DIRECTION('ref_axis',(1.,0.,0.));
#6171=DIRECTION('center_axis',(0.,1.,0.));
#6172=DIRECTION('ref_axis',(1.,0.,0.));
#6173=DIRECTION('',(0.,-1.,0.));
#6174=DIRECTION('center_axis',(0.,1.,0.));
#6175=DIRECTION('ref_axis',(1.,0.,0.));
#6176=DIRECTION('center_axis',(0.,1.,0.));
#6177=DIRECTION('ref_axis',(1.,0.,0.));
#6178=DIRECTION('center_axis',(0.,1.,0.));
#6179=DIRECTION('ref_axis',(1.,0.,0.));
#6180=DIRECTION('axis',(0.,0.,1.));
#6181=DIRECTION('refdir',(1.,0.,0.));
#6182=DIRECTION('center_axis',(0.,1.,0.));
#6183=DIRECTION('ref_axis',(1.,0.,0.));
#6184=DIRECTION('center_axis',(0.,-1.,0.));
#6185=DIRECTION('ref_axis',(1.,0.,0.));
#6186=DIRECTION('',(0.,-1.,0.));
#6187=DIRECTION('center_axis',(0.,-1.,0.));
#6188=DIRECTION('ref_axis',(1.,0.,0.));
#6189=DIRECTION('center_axis',(0.,1.,0.));
#6190=DIRECTION('ref_axis',(1.,0.,0.));
#6191=DIRECTION('center_axis',(0.,1.,0.));
#6192=DIRECTION('ref_axis',(1.,0.,0.));
#6193=DIRECTION('',(0.,-1.,0.));
#6194=DIRECTION('center_axis',(0.,1.,0.));
#6195=DIRECTION('ref_axis',(1.,0.,0.));
#6196=DIRECTION('center_axis',(0.,1.,0.));
#6197=DIRECTION('ref_axis',(1.,0.,0.));
#6198=DIRECTION('center_axis',(0.,1.,0.));
#6199=DIRECTION('ref_axis',(1.,0.,0.));
#6200=DIRECTION('axis',(0.,0.,1.));
#6201=DIRECTION('refdir',(1.,0.,0.));
#6202=DIRECTION('center_axis',(0.,1.,0.));
#6203=DIRECTION('ref_axis',(1.,0.,0.));
#6204=DIRECTION('center_axis',(0.,-1.,0.));
#6205=DIRECTION('ref_axis',(1.,0.,0.));
#6206=DIRECTION('',(0.,-1.,0.));
#6207=DIRECTION('center_axis',(0.,-1.,0.));
#6208=DIRECTION('ref_axis',(1.,0.,0.));
#6209=DIRECTION('center_axis',(0.,1.,0.));
#6210=DIRECTION('ref_axis',(1.,0.,0.));
#6211=DIRECTION('center_axis',(0.,1.,0.));
#6212=DIRECTION('ref_axis',(1.,0.,0.));
#6213=DIRECTION('',(0.,-1.,0.));
#6214=DIRECTION('center_axis',(0.,1.,0.));
#6215=DIRECTION('ref_axis',(1.,0.,0.));
#6216=DIRECTION('center_axis',(0.,1.,0.));
#6217=DIRECTION('ref_axis',(1.,0.,0.));
#6218=DIRECTION('center_axis',(0.,1.,0.));
#6219=DIRECTION('ref_axis',(1.,0.,0.));
#6220=DIRECTION('axis',(0.,0.,1.));
#6221=DIRECTION('refdir',(1.,0.,0.));
#6222=DIRECTION('center_axis',(0.,1.,0.));
#6223=DIRECTION('ref_axis',(1.,0.,0.));
#6224=DIRECTION('center_axis',(0.,-1.,0.));
#6225=DIRECTION('ref_axis',(1.,0.,0.));
#6226=DIRECTION('',(0.,-1.,0.));
#6227=DIRECTION('center_axis',(0.,-1.,0.));
#6228=DIRECTION('ref_axis',(1.,0.,0.));
#6229=DIRECTION('center_axis',(0.,1.,0.));
#6230=DIRECTION('ref_axis',(1.,0.,0.));
#6231=DIRECTION('center_axis',(0.,1.,0.));
#6232=DIRECTION('ref_axis',(1.,0.,0.));
#6233=DIRECTION('',(0.,-1.,0.));
#6234=DIRECTION('center_axis',(0.,1.,0.));
#6235=DIRECTION('ref_axis',(1.,0.,0.));
#6236=DIRECTION('center_axis',(0.,1.,0.));
#6237=DIRECTION('ref_axis',(1.,0.,0.));
#6238=DIRECTION('center_axis',(0.,1.,0.));
#6239=DIRECTION('ref_axis',(1.,0.,0.));
#6240=DIRECTION('axis',(0.,0.,1.));
#6241=DIRECTION('refdir',(1.,0.,0.));
#6242=DIRECTION('axis',(0.,0.,1.));
#6243=DIRECTION('refdir',(1.,0.,0.));
#6244=DIRECTION('center_axis',(0.,-1.,0.));
#6245=DIRECTION('ref_axis',(0.,0.,-1.));
#6246=DIRECTION('center_axis',(0.,-1.,0.));
#6247=DIRECTION('ref_axis',(1.,0.,0.));
#6248=DIRECTION('center_axis',(0.,-1.,0.));
#6249=DIRECTION('ref_axis',(1.,0.,0.));
#6250=DIRECTION('center_axis',(1.,0.,1.22464679914735E-16));
#6251=DIRECTION('ref_axis',(-1.22464679914735E-16,0.,1.));
#6252=DIRECTION('center_axis',(0.,1.,0.));
#6253=DIRECTION('ref_axis',(1.,0.,0.));
#6254=DIRECTION('center_axis',(0.,1.,0.));
#6255=DIRECTION('ref_axis',(1.,0.,0.));
#6256=DIRECTION('center_axis',(0.,-1.,0.));
#6257=DIRECTION('ref_axis',(1.,0.,0.));
#6258=DIRECTION('',(0.,1.,0.));
#6259=DIRECTION('center_axis',(0.,-1.,0.));
#6260=DIRECTION('ref_axis',(1.,0.,0.));
#6261=DIRECTION('center_axis',(0.,-1.,0.));
#6262=DIRECTION('ref_axis',(1.,0.,0.));
#6263=DIRECTION('center_axis',(0.,-1.,0.));
#6264=DIRECTION('ref_axis',(1.,0.,0.));
#6265=DIRECTION('',(0.,1.,0.));
#6266=DIRECTION('center_axis',(0.,-1.,0.));
#6267=DIRECTION('ref_axis',(1.,0.,0.));
#6268=DIRECTION('center_axis',(0.,1.,0.));
#6269=DIRECTION('ref_axis',(1.,0.,0.));
#6270=DIRECTION('',(-0.707106781186547,0.707106781186548,-8.65956056235493E-17));
#6271=DIRECTION('center_axis',(0.,-1.,0.));
#6272=DIRECTION('ref_axis',(1.,0.,0.));
#6273=DIRECTION('center_axis',(0.,1.,0.));
#6274=DIRECTION('ref_axis',(0.,0.,1.));
#6275=DIRECTION('center_axis',(0.,-1.,0.));
#6276=DIRECTION('ref_axis',(1.,0.,0.));
#6277=DIRECTION('center_axis',(0.,-1.,0.));
#6278=DIRECTION('ref_axis',(1.,0.,0.));
#6279=DIRECTION('',(0.,1.,0.));
#6280=DIRECTION('center_axis',(0.,-1.,0.));
#6281=DIRECTION('ref_axis',(0.,0.,-1.));
#6282=DIRECTION('center_axis',(0.,-1.,0.));
#6283=DIRECTION('ref_axis',(1.,0.,0.));
#6284=DIRECTION('center_axis',(0.,-1.,0.));
#6285=DIRECTION('ref_axis',(1.,0.,0.));
#6286=DIRECTION('',(0.707106781186547,0.707106781186548,8.65956056235493E-17));
#6287=DIRECTION('axis',(0.,0.,1.));
#6288=DIRECTION('refdir',(1.,0.,0.));
#6289=DIRECTION('center_axis',(0.,-1.,0.));
#6290=DIRECTION('ref_axis',(0.,0.,-1.));
#6291=DIRECTION('center_axis',(0.,-1.,0.));
#6292=DIRECTION('ref_axis',(1.,0.,0.));
#6293=DIRECTION('center_axis',(0.,-1.,0.));
#6294=DIRECTION('ref_axis',(1.,0.,0.));
#6295=DIRECTION('center_axis',(1.,0.,1.22464679914735E-16));
#6296=DIRECTION('ref_axis',(-1.22464679914735E-16,0.,1.));
#6297=DIRECTION('center_axis',(0.,1.,0.));
#6298=DIRECTION('ref_axis',(1.,0.,0.));
#6299=DIRECTION('center_axis',(0.,1.,0.));
#6300=DIRECTION('ref_axis',(1.,0.,0.));
#6301=DIRECTION('center_axis',(0.,-1.,0.));
#6302=DIRECTION('ref_axis',(1.,0.,0.));
#6303=DIRECTION('center_axis',(0.,-1.,0.));
#6304=DIRECTION('ref_axis',(1.,0.,0.));
#6305=DIRECTION('',(0.,1.,0.));
#6306=DIRECTION('center_axis',(0.,1.,0.));
#6307=DIRECTION('ref_axis',(0.,0.,1.));
#6308=DIRECTION('center_axis',(0.,-1.,0.));
#6309=DIRECTION('ref_axis',(1.,0.,0.));
#6310=DIRECTION('center_axis',(0.,-1.,0.));
#6311=DIRECTION('ref_axis',(1.,0.,0.));
#6312=DIRECTION('center_axis',(0.,-1.,0.));
#6313=DIRECTION('ref_axis',(1.,0.,0.));
#6314=DIRECTION('center_axis',(0.,-1.,0.));
#6315=DIRECTION('ref_axis',(1.,0.,0.));
#6316=DIRECTION('',(0.707106781186548,0.707106781186547,8.65956056235494E-17));
#6317=DIRECTION('center_axis',(0.,-1.,0.));
#6318=DIRECTION('ref_axis',(1.,0.,0.));
#6319=DIRECTION('center_axis',(0.,-1.,0.));
#6320=DIRECTION('ref_axis',(1.,0.,0.));
#6321=DIRECTION('',(0.,1.,0.));
#6322=DIRECTION('center_axis',(0.,1.,0.));
#6323=DIRECTION('ref_axis',(1.,0.,0.));
#6324=DIRECTION('center_axis',(0.,-1.,0.));
#6325=DIRECTION('ref_axis',(1.,0.,0.));
#6326=DIRECTION('',(-0.707106781186548,0.707106781186547,-8.65956056235494E-17));
#6327=DIRECTION('center_axis',(0.,-1.,0.));
#6328=DIRECTION('ref_axis',(0.,0.,-1.));
#6329=DIRECTION('center_axis',(0.,-1.,0.));
#6330=DIRECTION('ref_axis',(1.,0.,0.));
#6331=DIRECTION('',(0.,1.,0.));
#6332=DIRECTION('axis',(0.,0.,1.));
#6333=DIRECTION('refdir',(1.,0.,0.));
#6334=DIRECTION('center_axis',(0.,0.,1.));
#6335=DIRECTION('ref_axis',(1.,0.,0.));
#6336=DIRECTION('center_axis',(1.22464679914735E-16,-1.,0.));
#6337=DIRECTION('ref_axis',(-1.,-1.22464679914735E-16,0.));
#6338=DIRECTION('center_axis',(0.707106781186548,0.,0.707106781186548));
#6339=DIRECTION('ref_axis',(0.707106781186548,0.,-0.707106781186548));
#6340=DIRECTION('center_axis',(8.65956056235494E-17,-1.,-8.65956056235493E-17));
#6341=DIRECTION('ref_axis',(-0.707106781186547,-1.22464679914735E-16,0.707106781186547));
#6342=DIRECTION('center_axis',(1.,0.,0.));
#6343=DIRECTION('ref_axis',(6.12323399573676E-17,0.,-1.));
#6344=DIRECTION('center_axis',(7.49879891330929E-33,-1.,-1.22464679914735E-16));
#6345=DIRECTION('ref_axis',(-6.12323399573676E-17,-1.22464679914735E-16,
1.));
#6346=DIRECTION('center_axis',(0.707106781186548,0.,-0.707106781186548));
#6347=DIRECTION('ref_axis',(-0.707106781186548,0.,-0.707106781186548));
#6348=DIRECTION('center_axis',(-8.65956056235493E-17,-1.,-8.65956056235494E-17));
#6349=DIRECTION('ref_axis',(0.707106781186547,-1.22464679914735E-16,0.707106781186547));
#6350=DIRECTION('center_axis',(0.,0.,-1.));
#6351=DIRECTION('ref_axis',(-1.,0.,-1.22464679914735E-16));
#6352=DIRECTION('center_axis',(-1.22464679914735E-16,-1.,-1.49975978266186E-32));
#6353=DIRECTION('ref_axis',(1.,-1.22464679914735E-16,1.22464679914735E-16));
#6354=DIRECTION('center_axis',(-0.707106781186547,0.,-0.707106781186548));
#6355=DIRECTION('ref_axis',(-0.707106781186548,0.,0.707106781186547));
#6356=DIRECTION('center_axis',(-8.65956056235493E-17,-1.,8.65956056235493E-17));
#6357=DIRECTION('ref_axis',(0.707106781186548,-1.22464679914735E-16,-0.707106781186547));
#6358=DIRECTION('center_axis',(-1.,0.,0.));
#6359=DIRECTION('ref_axis',(-1.83697019872103E-16,0.,1.));
#6360=DIRECTION('center_axis',(-2.24963967399279E-32,-1.,1.22464679914735E-16));
#6361=DIRECTION('ref_axis',(1.83697019872103E-16,-1.22464679914735E-16,
-1.));
#6362=DIRECTION('center_axis',(-0.707106781186548,0.,0.707106781186548));
#6363=DIRECTION('ref_axis',(0.707106781186547,0.,0.707106781186548));
#6364=DIRECTION('center_axis',(8.65956056235493E-17,-1.,8.65956056235493E-17));
#6365=DIRECTION('ref_axis',(-0.707106781186547,-1.22464679914735E-16,-0.707106781186548));
#6366=DIRECTION('axis',(0.,0.,1.));
#6367=DIRECTION('refdir',(1.,0.,0.));
#6368=DIRECTION('center_axis',(0.,0.,1.));
#6369=DIRECTION('ref_axis',(1.,0.,0.));
#6370=DIRECTION('center_axis',(0.,-1.,0.));
#6371=DIRECTION('ref_axis',(0.,0.,-1.));
#6372=DIRECTION('center_axis',(0.,-1.,0.));
#6373=DIRECTION('ref_axis',(0.,0.,-1.));
#6374=DIRECTION('center_axis',(0.,1.,0.));
#6375=DIRECTION('ref_axis',(1.,0.,0.));
#6376=DIRECTION('center_axis',(0.,1.,0.));
#6377=DIRECTION('ref_axis',(1.,0.,0.));
#6378=DIRECTION('center_axis',(0.,1.,0.));
#6379=DIRECTION('ref_axis',(1.,0.,0.));
#6380=DIRECTION('center_axis',(0.,1.,0.));
#6381=DIRECTION('ref_axis',(1.,0.,0.));
#6382=DIRECTION('',(0.,-1.,0.));
#6383=DIRECTION('center_axis',(0.,-1.,0.));
#6384=DIRECTION('ref_axis',(1.,0.,0.));
#6385=DIRECTION('center_axis',(0.,1.,0.));
#6386=DIRECTION('ref_axis',(1.,0.,0.));
#6387=DIRECTION('center_axis',(0.,1.,0.));
#6388=DIRECTION('ref_axis',(1.,0.,0.));
#6389=DIRECTION('center_axis',(0.,1.,0.));
#6390=DIRECTION('ref_axis',(1.,0.,0.));
#6391=DIRECTION('center_axis',(0.,1.,0.));
#6392=DIRECTION('ref_axis',(1.,0.,0.));
#6393=DIRECTION('center_axis',(0.,1.,0.));
#6394=DIRECTION('ref_axis',(1.,0.,0.));
#6395=DIRECTION('center_axis',(0.,1.,0.));
#6396=DIRECTION('ref_axis',(1.,0.,0.));
#6397=DIRECTION('center_axis',(0.,-1.,0.));
#6398=DIRECTION('ref_axis',(1.,0.,0.));
#6399=DIRECTION('center_axis',(0.,-1.,0.));
#6400=DIRECTION('ref_axis',(0.,0.,-1.));
#6401=DIRECTION('center_axis',(6.12323399573677E-17,0.,1.));
#6402=DIRECTION('ref_axis',(1.,0.,0.));
#6403=DIRECTION('center_axis',(0.,-1.,0.));
#6404=DIRECTION('ref_axis',(0.,0.,-1.));
#6405=DIRECTION('center_axis',(0.,1.,0.));
#6406=DIRECTION('ref_axis',(1.,0.,0.));
#6407=DIRECTION('center_axis',(0.,-1.,0.));
#6408=DIRECTION('ref_axis',(1.,0.,0.));
#6409=DIRECTION('center_axis',(0.,-1.,0.));
#6410=DIRECTION('ref_axis',(0.,0.,-1.));
#6411=DIRECTION('center_axis',(0.,0.,1.));
#6412=DIRECTION('ref_axis',(1.,0.,0.));
#6413=DIRECTION('center_axis',(0.,-1.,0.));
#6414=DIRECTION('ref_axis',(0.,0.,-1.));
#6415=DIRECTION('center_axis',(0.,1.,0.));
#6416=DIRECTION('ref_axis',(1.,0.,0.));
#6417=DIRECTION('center_axis',(0.,-1.,0.));
#6418=DIRECTION('ref_axis',(1.,0.,0.));
#6419=DIRECTION('center_axis',(0.,-1.,0.));
#6420=DIRECTION('ref_axis',(0.,0.,-1.));
#6421=DIRECTION('center_axis',(0.,0.,1.));
#6422=DIRECTION('ref_axis',(1.,0.,0.));
#6423=DIRECTION('center_axis',(0.,-1.,0.));
#6424=DIRECTION('ref_axis',(0.,0.,-1.));
#6425=DIRECTION('center_axis',(0.,1.,0.));
#6426=DIRECTION('ref_axis',(1.,0.,0.));
#6427=DIRECTION('center_axis',(0.,-1.,0.));
#6428=DIRECTION('ref_axis',(1.,0.,0.));
#6429=DIRECTION('center_axis',(0.,-1.,0.));
#6430=DIRECTION('ref_axis',(0.,0.,-1.));
#6431=DIRECTION('center_axis',(0.,0.,1.));
#6432=DIRECTION('ref_axis',(1.,0.,0.));
#6433=DIRECTION('center_axis',(0.,-1.,0.));
#6434=DIRECTION('ref_axis',(0.,0.,-1.));
#6435=DIRECTION('center_axis',(0.,1.,0.));
#6436=DIRECTION('ref_axis',(1.,0.,0.));
#6437=DIRECTION('center_axis',(0.,-1.,0.));
#6438=DIRECTION('ref_axis',(1.,0.,0.));
#6439=DIRECTION('center_axis',(0.,-1.,0.));
#6440=DIRECTION('ref_axis',(0.,0.,-1.));
#6441=DIRECTION('center_axis',(6.12323399573676E-17,0.,1.));
#6442=DIRECTION('ref_axis',(1.,0.,0.));
#6443=DIRECTION('center_axis',(0.,-1.,0.));
#6444=DIRECTION('ref_axis',(0.,0.,-1.));
#6445=DIRECTION('center_axis',(0.,1.,0.));
#6446=DIRECTION('ref_axis',(1.,0.,0.));
#6447=DIRECTION('center_axis',(0.,-1.,0.));
#6448=DIRECTION('ref_axis',(1.,0.,0.));
#6449=DIRECTION('center_axis',(0.,-1.,0.));
#6450=DIRECTION('ref_axis',(0.,0.,-1.));
#6451=DIRECTION('center_axis',(0.,0.,1.));
#6452=DIRECTION('ref_axis',(1.,0.,0.));
#6453=DIRECTION('center_axis',(0.,-1.,0.));
#6454=DIRECTION('ref_axis',(0.,0.,-1.));
#6455=DIRECTION('center_axis',(0.,1.,0.));
#6456=DIRECTION('ref_axis',(1.,0.,0.));
#6457=DIRECTION('center_axis',(0.,1.,0.));
#6458=DIRECTION('ref_axis',(1.,0.,0.));
#6459=DIRECTION('',(0.,1.,0.));
#6460=DIRECTION('center_axis',(0.,-1.,0.));
#6461=DIRECTION('ref_axis',(1.,0.,0.));
#6462=DIRECTION('center_axis',(0.,-1.,0.));
#6463=DIRECTION('ref_axis',(1.,0.,0.));
#6464=DIRECTION('center_axis',(0.,1.,0.));
#6465=DIRECTION('ref_axis',(1.,0.,0.));
#6466=DIRECTION('center_axis',(0.,-1.,0.));
#6467=DIRECTION('ref_axis',(0.,0.,-1.));
#6468=DIRECTION('center_axis',(0.,0.,1.));
#6469=DIRECTION('ref_axis',(1.,0.,0.));
#6470=DIRECTION('center_axis',(0.,-1.,0.));
#6471=DIRECTION('ref_axis',(0.,0.,-1.));
#6472=DIRECTION('center_axis',(0.,-1.,0.));
#6473=DIRECTION('ref_axis',(-1.,0.,0.));
#6474=DIRECTION('center_axis',(0.,1.,0.));
#6475=DIRECTION('ref_axis',(1.,0.,0.));
#6476=DIRECTION('axis',(0.,0.,1.));
#6477=DIRECTION('refdir',(1.,0.,0.));
#6478=DIRECTION('center_axis',(0.,1.,0.));
#6479=DIRECTION('ref_axis',(0.,0.,1.));
#6480=DIRECTION('center_axis',(0.,-1.,0.));
#6481=DIRECTION('ref_axis',(1.,0.,0.));
#6482=DIRECTION('center_axis',(0.,-1.,0.));
#6483=DIRECTION('ref_axis',(1.,0.,0.));
#6484=DIRECTION('center_axis',(0.,-1.,0.));
#6485=DIRECTION('ref_axis',(1.,0.,0.));
#6486=DIRECTION('center_axis',(0.,-1.,0.));
#6487=DIRECTION('ref_axis',(1.,0.,0.));
#6488=DIRECTION('',(0.,1.,0.));
#6489=DIRECTION('center_axis',(0.,-1.,0.));
#6490=DIRECTION('ref_axis',(0.,0.,-1.));
#6491=DIRECTION('center_axis',(0.,-1.,0.));
#6492=DIRECTION('ref_axis',(1.,0.,0.));
#6493=DIRECTION('center_axis',(0.,-1.,0.));
#6494=DIRECTION('ref_axis',(1.,0.,0.));
#6495=DIRECTION('',(0.,1.,0.));
#6496=DIRECTION('center_axis',(0.,1.,0.));
#6497=DIRECTION('ref_axis',(0.,0.,1.));
#6498=DIRECTION('center_axis',(0.,-1.,0.));
#6499=DIRECTION('ref_axis',(1.,0.,0.));
#6500=DIRECTION('center_axis',(0.,-1.,0.));
#6501=DIRECTION('ref_axis',(1.,0.,0.));
#6502=DIRECTION('center_axis',(0.,-1.,0.));
#6503=DIRECTION('ref_axis',(1.,0.,0.));
#6504=DIRECTION('center_axis',(0.,-1.,0.));
#6505=DIRECTION('ref_axis',(1.,0.,0.));
#6506=DIRECTION('',(0.,1.,0.));
#6507=DIRECTION('center_axis',(0.,-1.,0.));
#6508=DIRECTION('ref_axis',(0.,0.,-1.));
#6509=DIRECTION('center_axis',(0.,-1.,0.));
#6510=DIRECTION('ref_axis',(1.,0.,0.));
#6511=DIRECTION('center_axis',(0.,-1.,0.));
#6512=DIRECTION('ref_axis',(1.,0.,0.));
#6513=DIRECTION('',(0.,1.,0.));
#6514=DIRECTION('',(0.,0.,1.));
#6515=DIRECTION('',(1.,0.,0.));
#6516=DIRECTION('',(0.,0.,1.));
#6517=DIRECTION('',(1.,0.,0.));
#6518=DIRECTION('',(0.,0.,1.));
#6519=DIRECTION('',(1.,0.,0.));
#6520=DIRECTION('',(0.,0.,1.));
#6521=DIRECTION('',(1.,0.,0.));
#6522=DIRECTION('',(0.,0.,1.));
#6523=DIRECTION('',(1.,0.,0.));
#6524=DIRECTION('axis',(0.,0.,1.));
#6525=DIRECTION('refdir',(1.,0.,0.));
#6526=DIRECTION('center_axis',(0.,0.,1.));
#6527=DIRECTION('ref_axis',(1.,0.,0.));
#6528=DIRECTION('',(0.,0.,-1.));
#6529=DIRECTION('center_axis',(0.,0.,-1.));
#6530=DIRECTION('ref_axis',(1.,0.,0.));
#6531=DIRECTION('',(0.,0.,1.));
#6532=DIRECTION('center_axis',(0.,0.,1.));
#6533=DIRECTION('ref_axis',(1.,0.,0.));
#6534=DIRECTION('center_axis',(0.,0.,1.));
#6535=DIRECTION('ref_axis',(-1.,-1.01064309961486E-15,0.));
#6536=DIRECTION('',(0.,0.,1.));
#6537=DIRECTION('center_axis',(0.,0.,1.));
#6538=DIRECTION('ref_axis',(1.,0.,0.));
#6539=DIRECTION('',(0.,0.,-1.));
#6540=DIRECTION('center_axis',(0.,0.,-1.));
#6541=DIRECTION('ref_axis',(1.,0.,0.));
#6542=DIRECTION('center_axis',(0.,1.,0.));
#6543=DIRECTION('ref_axis',(1.,0.,0.));
#6544=DIRECTION('',(-1.,0.,0.));
#6545=DIRECTION('',(0.,0.,1.));
#6546=DIRECTION('',(-1.,0.,0.));
#6547=DIRECTION('center_axis',(0.,1.,0.));
#6548=DIRECTION('ref_axis',(1.,0.,0.));
#6549=DIRECTION('',(-1.,0.,0.));
#6550=DIRECTION('',(0.,0.,-1.));
#6551=DIRECTION('',(-1.,0.,0.));
#6552=DIRECTION('center_axis',(0.,1.,0.));
#6553=DIRECTION('ref_axis',(1.,0.,0.));
#6554=DIRECTION('center_axis',(0.,0.,1.));
#6555=DIRECTION('ref_axis',(1.,0.,0.));
#6556=DIRECTION('',(0.,1.,0.));
#6557=DIRECTION('',(1.,0.,0.));
#6558=DIRECTION('center_axis',(0.,0.,1.));
#6559=DIRECTION('ref_axis',(1.,0.,0.));
#6560=DIRECTION('',(1.,0.,0.));
#6561=DIRECTION('center_axis',(0.,0.,-1.));
#6562=DIRECTION('ref_axis',(1.,0.,0.));
#6563=DIRECTION('center_axis',(0.,1.,0.));
#6564=DIRECTION('ref_axis',(0.,0.,1.));
#6565=DIRECTION('',(0.,0.,-1.));
#6566=DIRECTION('',(1.,0.,0.));
#6567=DIRECTION('center_axis',(0.,1.,0.));
#6568=DIRECTION('ref_axis',(0.,0.,1.));
#6569=DIRECTION('',(1.,0.,0.));
#6570=DIRECTION('',(0.,0.,1.));
#6571=DIRECTION('center_axis',(0.,-1.,0.));
#6572=DIRECTION('ref_axis',(1.,0.,0.));
#6573=DIRECTION('center_axis',(0.,0.,1.));
#6574=DIRECTION('ref_axis',(1.,0.,0.));
#6575=DIRECTION('center_axis',(0.,0.,1.));
#6576=DIRECTION('ref_axis',(1.,0.,0.));
#6577=DIRECTION('',(0.,0.,1.));
#6578=DIRECTION('center_axis',(0.,0.,1.));
#6579=DIRECTION('ref_axis',(1.,0.,0.));
#6580=DIRECTION('center_axis',(0.,0.,1.));
#6581=DIRECTION('ref_axis',(-1.,-7.6571373978539E-16,0.));
#6582=DIRECTION('',(0.,0.,-1.));
#6583=DIRECTION('center_axis',(0.,0.,-1.));
#6584=DIRECTION('ref_axis',(1.,0.,0.));
#6585=DIRECTION('',(0.,0.,1.));
#6586=DIRECTION('center_axis',(0.,0.,1.));
#6587=DIRECTION('ref_axis',(1.,0.,0.));
#6588=DIRECTION('center_axis',(0.,0.,1.));
#6589=DIRECTION('ref_axis',(1.,0.,0.));
#6590=DIRECTION('center_axis',(0.,0.,1.));
#6591=DIRECTION('ref_axis',(1.,0.,0.));
#6592=DIRECTION('center_axis',(0.,1.,0.));
#6593=DIRECTION('ref_axis',(0.,0.,1.));
#6594=DIRECTION('',(1.,0.,0.));
#6595=DIRECTION('',(0.,0.,1.));
#6596=DIRECTION('',(1.,0.,0.));
#6597=DIRECTION('center_axis',(0.,0.,1.));
#6598=DIRECTION('ref_axis',(1.,0.,0.));
#6599=DIRECTION('',(0.,1.,0.));
#6600=DIRECTION('',(-1.,0.,0.));
#6601=DIRECTION('center_axis',(0.,1.,0.));
#6602=DIRECTION('ref_axis',(1.,0.,0.));
#6603=DIRECTION('',(0.,0.,-1.));
#6604=DIRECTION('',(-1.,0.,0.));
#6605=DIRECTION('center_axis',(0.,0.,1.));
#6606=DIRECTION('ref_axis',(1.,0.,0.));
#6607=DIRECTION('center_axis',(0.,0.,1.));
#6608=DIRECTION('ref_axis',(1.,0.,0.));
#6609=DIRECTION('',(0.,0.,1.));
#6610=DIRECTION('center_axis',(0.,0.,1.));
#6611=DIRECTION('ref_axis',(1.,0.,0.));
#6612=DIRECTION('center_axis',(0.,1.,0.));
#6613=DIRECTION('ref_axis',(1.,0.,0.));
#6614=DIRECTION('',(0.,1.,0.));
#6615=DIRECTION('center_axis',(1.,0.,0.));
#6616=DIRECTION('ref_axis',(0.,0.,-1.));
#6617=DIRECTION('',(0.,-1.,0.));
#6618=DIRECTION('center_axis',(-1.,0.,0.));
#6619=DIRECTION('ref_axis',(0.,0.,1.));
#6620=DIRECTION('',(0.,1.,0.));
#6621=DIRECTION('center_axis',(0.,1.,0.));
#6622=DIRECTION('ref_axis',(-1.,0.,0.));
#6623=DIRECTION('',(-1.,0.,0.));
#6624=DIRECTION('',(0.,0.,1.));
#6625=DIRECTION('',(-1.,0.,0.));
#6626=DIRECTION('',(0.,0.,1.));
#6627=DIRECTION('center_axis',(1.,0.,0.));
#6628=DIRECTION('ref_axis',(0.,1.,0.));
#6629=DIRECTION('',(0.,1.,0.));
#6630=DIRECTION('',(0.,1.,0.));
#6631=DIRECTION('',(0.,0.,1.));
#6632=DIRECTION('center_axis',(0.,-1.,0.));
#6633=DIRECTION('ref_axis',(1.,0.,0.));
#6634=DIRECTION('',(1.,0.,0.));
#6635=DIRECTION('',(1.,0.,0.));
#6636=DIRECTION('',(0.,0.,1.));
#6637=DIRECTION('center_axis',(-1.,0.,0.));
#6638=DIRECTION('ref_axis',(0.,-1.,0.));
#6639=DIRECTION('',(0.,-1.,0.));
#6640=DIRECTION('',(0.,-1.,0.));
#6641=DIRECTION('center_axis',(0.,0.,1.));
#6642=DIRECTION('ref_axis',(1.,0.,0.));
#6643=DIRECTION('center_axis',(0.,0.,1.));
#6644=DIRECTION('ref_axis',(1.,0.,0.));
#6645=DIRECTION('axis',(0.,0.,1.));
#6646=DIRECTION('refdir',(1.,0.,0.));
#6647=DIRECTION('center_axis',(0.,0.,1.));
#6648=DIRECTION('ref_axis',(1.,0.,0.));
#6649=DIRECTION('center_axis',(0.,0.,1.));
#6650=DIRECTION('ref_axis',(1.,0.,0.));
#6651=DIRECTION('',(0.,0.,1.));
#6652=DIRECTION('center_axis',(0.,0.,-1.));
#6653=DIRECTION('ref_axis',(1.,0.,0.));
#6654=DIRECTION('center_axis',(1.,0.,0.));
#6655=DIRECTION('ref_axis',(0.,0.,-1.));
#6656=DIRECTION('center_axis',(1.,0.,0.));
#6657=DIRECTION('ref_axis',(0.,0.,-1.));
#6658=DIRECTION('',(1.,0.,0.));
#6659=DIRECTION('center_axis',(-1.,0.,0.));
#6660=DIRECTION('ref_axis',(0.,0.,-1.));
#6661=DIRECTION('center_axis',(0.,0.,1.));
#6662=DIRECTION('ref_axis',(0.,-1.,0.));
#6663=DIRECTION('',(0.,-1.,0.));
#6664=DIRECTION('',(1.,0.,0.));
#6665=DIRECTION('',(0.,-1.,0.));
#6666=DIRECTION('',(1.,0.,0.));
#6667=DIRECTION('center_axis',(1.,0.,0.));
#6668=DIRECTION('ref_axis',(0.,0.,-1.));
#6669=DIRECTION('',(0.,-1.,0.));
#6670=DIRECTION('',(0.,0.,1.));
#6671=DIRECTION('',(0.,0.,-1.));
#6672=DIRECTION('center_axis',(0.,0.,1.));
#6673=DIRECTION('ref_axis',(1.,0.,0.));
#6674=DIRECTION('',(1.,0.,0.));
#6675=DIRECTION('',(0.,1.,0.));
#6676=DIRECTION('',(-1.,0.,0.));
#6677=DIRECTION('center_axis',(0.,-1.,0.));
#6678=DIRECTION('ref_axis',(1.,0.,0.));
#6679=DIRECTION('',(0.,0.,1.));
#6680=DIRECTION('',(1.,0.,0.));
#6681=DIRECTION('',(0.,0.,1.));
#6682=DIRECTION('center_axis',(0.,1.,0.));
#6683=DIRECTION('ref_axis',(-1.,0.,0.));
#6684=DIRECTION('',(0.,0.,1.));
#6685=DIRECTION('',(-1.,0.,0.));
#6686=DIRECTION('',(0.,0.,1.));
#6687=DIRECTION('center_axis',(1.,0.,0.));
#6688=DIRECTION('ref_axis',(0.,1.,0.));
#6689=DIRECTION('',(0.,1.,0.));
#6690=DIRECTION('center_axis',(-1.,0.,0.));
#6691=DIRECTION('ref_axis',(0.,-1.,0.));
#6692=DIRECTION('',(0.,-1.,0.));
#6693=DIRECTION('center_axis',(0.,0.,1.));
#6694=DIRECTION('ref_axis',(1.,0.,0.));
#6695=DIRECTION('axis',(0.,0.,1.));
#6696=DIRECTION('refdir',(1.,0.,0.));
#6697=DIRECTION('center_axis',(0.,0.,1.));
#6698=DIRECTION('ref_axis',(1.,0.,0.));
#6699=DIRECTION('',(0.,0.,-1.));
#6700=DIRECTION('center_axis',(0.,0.,-1.));
#6701=DIRECTION('ref_axis',(1.,0.,0.));
#6702=DIRECTION('',(0.,0.,1.));
#6703=DIRECTION('center_axis',(0.,0.,1.));
#6704=DIRECTION('ref_axis',(1.,0.,0.));
#6705=DIRECTION('center_axis',(0.,0.,1.));
#6706=DIRECTION('ref_axis',(-1.,-1.22464679914735E-16,0.));
#6707=DIRECTION('',(0.,0.,1.));
#6708=DIRECTION('center_axis',(0.,0.,1.));
#6709=DIRECTION('ref_axis',(1.,0.,0.));
#6710=DIRECTION('',(0.,0.,-1.));
#6711=DIRECTION('center_axis',(0.,0.,-1.));
#6712=DIRECTION('ref_axis',(1.,0.,0.));
#6713=DIRECTION('center_axis',(0.,1.,0.));
#6714=DIRECTION('ref_axis',(1.,0.,0.));
#6715=DIRECTION('',(-1.,0.,0.));
#6716=DIRECTION('',(0.,0.,1.));
#6717=DIRECTION('',(-1.,0.,0.));
#6718=DIRECTION('center_axis',(0.,1.,0.));
#6719=DIRECTION('ref_axis',(1.,0.,0.));
#6720=DIRECTION('',(-1.,0.,0.));
#6721=DIRECTION('',(0.,0.,-1.));
#6722=DIRECTION('',(-1.,0.,0.));
#6723=DIRECTION('center_axis',(0.,1.,0.));
#6724=DIRECTION('ref_axis',(1.,0.,0.));
#6725=DIRECTION('center_axis',(0.,0.,1.));
#6726=DIRECTION('ref_axis',(1.,0.,0.));
#6727=DIRECTION('',(0.,1.,0.));
#6728=DIRECTION('',(1.,0.,0.));
#6729=DIRECTION('center_axis',(0.,0.,1.));
#6730=DIRECTION('ref_axis',(1.,0.,0.));
#6731=DIRECTION('',(1.,0.,0.));
#6732=DIRECTION('center_axis',(0.,0.,-1.));
#6733=DIRECTION('ref_axis',(1.,0.,0.));
#6734=DIRECTION('center_axis',(0.,1.,0.));
#6735=DIRECTION('ref_axis',(0.,0.,1.));
#6736=DIRECTION('',(0.,0.,-1.));
#6737=DIRECTION('',(1.,0.,0.));
#6738=DIRECTION('center_axis',(0.,1.,0.));
#6739=DIRECTION('ref_axis',(0.,0.,1.));
#6740=DIRECTION('',(1.,0.,0.));
#6741=DIRECTION('',(0.,0.,1.));
#6742=DIRECTION('center_axis',(0.,-1.,0.));
#6743=DIRECTION('ref_axis',(1.,0.,0.));
#6744=DIRECTION('center_axis',(0.,0.,1.));
#6745=DIRECTION('ref_axis',(1.,0.,0.));
#6746=DIRECTION('center_axis',(0.,0.,1.));
#6747=DIRECTION('ref_axis',(1.,0.,0.));
#6748=DIRECTION('',(0.,0.,1.));
#6749=DIRECTION('center_axis',(0.,0.,1.));
#6750=DIRECTION('ref_axis',(1.,0.,0.));
#6751=DIRECTION('center_axis',(0.,0.,1.));
#6752=DIRECTION('ref_axis',(-1.,1.22464679914735E-16,0.));
#6753=DIRECTION('',(0.,0.,-1.));
#6754=DIRECTION('center_axis',(0.,0.,-1.));
#6755=DIRECTION('ref_axis',(1.,0.,0.));
#6756=DIRECTION('',(0.,0.,1.));
#6757=DIRECTION('center_axis',(0.,0.,1.));
#6758=DIRECTION('ref_axis',(1.,0.,0.));
#6759=DIRECTION('center_axis',(0.,0.,1.));
#6760=DIRECTION('ref_axis',(1.,0.,0.));
#6761=DIRECTION('center_axis',(0.,0.,1.));
#6762=DIRECTION('ref_axis',(1.,0.,0.));
#6763=DIRECTION('center_axis',(0.,1.,0.));
#6764=DIRECTION('ref_axis',(0.,0.,1.));
#6765=DIRECTION('',(1.,0.,0.));
#6766=DIRECTION('',(0.,0.,1.));
#6767=DIRECTION('',(1.,0.,0.));
#6768=DIRECTION('center_axis',(0.,0.,1.));
#6769=DIRECTION('ref_axis',(1.,0.,0.));
#6770=DIRECTION('',(0.,1.,0.));
#6771=DIRECTION('',(-1.,0.,0.));
#6772=DIRECTION('center_axis',(0.,1.,0.));
#6773=DIRECTION('ref_axis',(1.,0.,0.));
#6774=DIRECTION('',(0.,0.,-1.));
#6775=DIRECTION('',(-1.,0.,0.));
#6776=DIRECTION('center_axis',(0.,0.,1.));
#6777=DIRECTION('ref_axis',(1.,0.,0.));
#6778=DIRECTION('center_axis',(0.,0.,1.));
#6779=DIRECTION('ref_axis',(1.,0.,0.));
#6780=DIRECTION('',(0.,0.,1.));
#6781=DIRECTION('center_axis',(0.,0.,1.));
#6782=DIRECTION('ref_axis',(1.,0.,0.));
#6783=DIRECTION('center_axis',(0.,1.,0.));
#6784=DIRECTION('ref_axis',(1.,0.,0.));
#6785=DIRECTION('',(0.,1.,0.));
#6786=DIRECTION('center_axis',(1.,0.,0.));
#6787=DIRECTION('ref_axis',(0.,0.,-1.));
#6788=DIRECTION('',(0.,-1.,0.));
#6789=DIRECTION('center_axis',(-1.,0.,0.));
#6790=DIRECTION('ref_axis',(0.,0.,1.));
#6791=DIRECTION('',(0.,1.,0.));
#6792=DIRECTION('center_axis',(0.,1.,0.));
#6793=DIRECTION('ref_axis',(-1.,0.,0.));
#6794=DIRECTION('',(-1.,0.,0.));
#6795=DIRECTION('',(0.,0.,1.));
#6796=DIRECTION('',(-1.,0.,0.));
#6797=DIRECTION('',(0.,0.,1.));
#6798=DIRECTION('center_axis',(1.,0.,0.));
#6799=DIRECTION('ref_axis',(0.,1.,0.));
#6800=DIRECTION('',(0.,1.,0.));
#6801=DIRECTION('',(0.,1.,0.));
#6802=DIRECTION('',(0.,0.,1.));
#6803=DIRECTION('center_axis',(0.,-1.,0.));
#6804=DIRECTION('ref_axis',(1.,0.,0.));
#6805=DIRECTION('',(1.,0.,0.));
#6806=DIRECTION('',(1.,0.,0.));
#6807=DIRECTION('',(0.,0.,1.));
#6808=DIRECTION('center_axis',(-1.,0.,0.));
#6809=DIRECTION('ref_axis',(0.,-1.,0.));
#6810=DIRECTION('',(0.,-1.,0.));
#6811=DIRECTION('',(0.,-1.,0.));
#6812=DIRECTION('center_axis',(0.,0.,1.));
#6813=DIRECTION('ref_axis',(1.,0.,0.));
#6814=DIRECTION('center_axis',(0.,0.,1.));
#6815=DIRECTION('ref_axis',(1.,0.,0.));
#6816=DIRECTION('axis',(0.,0.,1.));
#6817=DIRECTION('refdir',(1.,0.,0.));
#6818=DIRECTION('center_axis',(0.,0.,1.));
#6819=DIRECTION('ref_axis',(1.,0.,0.));
#6820=DIRECTION('center_axis',(0.,0.,1.));
#6821=DIRECTION('ref_axis',(1.,0.,0.));
#6822=DIRECTION('',(0.,0.,1.));
#6823=DIRECTION('center_axis',(0.,0.,-1.));
#6824=DIRECTION('ref_axis',(1.,0.,0.));
#6825=DIRECTION('center_axis',(1.,0.,0.));
#6826=DIRECTION('ref_axis',(0.,0.,-1.));
#6827=DIRECTION('center_axis',(1.,0.,0.));
#6828=DIRECTION('ref_axis',(0.,0.,-1.));
#6829=DIRECTION('',(1.,0.,0.));
#6830=DIRECTION('center_axis',(-1.,0.,0.));
#6831=DIRECTION('ref_axis',(0.,0.,-1.));
#6832=DIRECTION('center_axis',(0.,0.,1.));
#6833=DIRECTION('ref_axis',(0.,-1.,0.));
#6834=DIRECTION('',(0.,-1.,0.));
#6835=DIRECTION('',(1.,0.,0.));
#6836=DIRECTION('',(0.,-1.,0.));
#6837=DIRECTION('',(1.,0.,0.));
#6838=DIRECTION('center_axis',(1.,0.,0.));
#6839=DIRECTION('ref_axis',(0.,0.,-1.));
#6840=DIRECTION('',(0.,-1.,0.));
#6841=DIRECTION('',(0.,0.,1.));
#6842=DIRECTION('',(0.,0.,-1.));
#6843=DIRECTION('center_axis',(0.,0.,1.));
#6844=DIRECTION('ref_axis',(1.,0.,0.));
#6845=DIRECTION('',(1.,0.,0.));
#6846=DIRECTION('',(0.,1.,0.));
#6847=DIRECTION('',(-1.,0.,0.));
#6848=DIRECTION('center_axis',(0.,-1.,0.));
#6849=DIRECTION('ref_axis',(1.,0.,0.));
#6850=DIRECTION('',(0.,0.,1.));
#6851=DIRECTION('',(1.,0.,0.));
#6852=DIRECTION('',(0.,0.,1.));
#6853=DIRECTION('center_axis',(0.,1.,0.));
#6854=DIRECTION('ref_axis',(-1.,0.,0.));
#6855=DIRECTION('',(0.,0.,1.));
#6856=DIRECTION('',(-1.,0.,0.));
#6857=DIRECTION('',(0.,0.,1.));
#6858=DIRECTION('center_axis',(1.,0.,0.));
#6859=DIRECTION('ref_axis',(0.,1.,0.));
#6860=DIRECTION('',(0.,1.,0.));
#6861=DIRECTION('center_axis',(-1.,0.,0.));
#6862=DIRECTION('ref_axis',(0.,-1.,0.));
#6863=DIRECTION('',(0.,-1.,0.));
#6864=DIRECTION('center_axis',(0.,0.,1.));
#6865=DIRECTION('ref_axis',(1.,0.,0.));
#6866=DIRECTION('axis',(0.,0.,1.));
#6867=DIRECTION('refdir',(1.,0.,0.));
#6868=DIRECTION('center_axis',(0.,0.,-1.));
#6869=DIRECTION('ref_axis',(0.,1.,0.));
#6870=DIRECTION('',(0.,1.,0.));
#6871=DIRECTION('',(1.,0.,0.));
#6872=DIRECTION('',(0.,-1.,0.));
#6873=DIRECTION('',(1.,0.,0.));
#6874=DIRECTION('center_axis',(0.,1.,-8.88178419700125E-16));
#6875=DIRECTION('ref_axis',(0.,8.88178419700125E-16,1.));
#6876=DIRECTION('',(0.,8.88178419700125E-16,1.));
#6877=DIRECTION('',(1.,0.,0.));
#6878=DIRECTION('',(0.,-8.88178419700125E-16,-1.));
#6879=DIRECTION('center_axis',(0.,-7.40148683083439E-16,-1.));
#6880=DIRECTION('ref_axis',(0.,1.,-7.40148683083439E-16));
#6881=DIRECTION('',(0.,1.,-7.40148683083439E-16));
#6882=DIRECTION('',(1.,0.,0.));
#6883=DIRECTION('',(0.,-1.,7.40148683083439E-16));
#6884=DIRECTION('center_axis',(0.,-0.707106781186547,-0.707106781186548));
#6885=DIRECTION('ref_axis',(0.,0.707106781186548,-0.707106781186547));
#6886=DIRECTION('',(0.,0.707106781186548,-0.707106781186547));
#6887=DIRECTION('',(1.,0.,0.));
#6888=DIRECTION('',(0.,-0.707106781186548,0.707106781186547));
#6889=DIRECTION('center_axis',(0.,-1.,2.77555756156289E-16));
#6890=DIRECTION('ref_axis',(0.,-2.77555756156289E-16,-1.));
#6891=DIRECTION('',(0.,-2.77555756156289E-16,-1.));
#6892=DIRECTION('',(1.,0.,0.));
#6893=DIRECTION('',(0.,2.77555756156289E-16,1.));
#6894=DIRECTION('center_axis',(0.,-0.707106781186547,0.707106781186548));
#6895=DIRECTION('ref_axis',(0.,-0.707106781186548,-0.707106781186547));
#6896=DIRECTION('',(0.,-0.707106781186548,-0.707106781186547));
#6897=DIRECTION('',(1.,0.,0.));
#6898=DIRECTION('',(0.,0.707106781186548,0.707106781186547));
#6899=DIRECTION('center_axis',(0.,7.40148683083438E-16,1.));
#6900=DIRECTION('ref_axis',(0.,-1.,7.40148683083438E-16));
#6901=DIRECTION('',(0.,-1.,7.40148683083438E-16));
#6902=DIRECTION('',(1.,0.,0.));
#6903=DIRECTION('',(0.,1.,-7.40148683083438E-16));
#6904=DIRECTION('center_axis',(0.,1.,-4.44089209850063E-16));
#6905=DIRECTION('ref_axis',(0.,4.44089209850063E-16,1.));
#6906=DIRECTION('',(0.,4.44089209850063E-16,1.));
#6907=DIRECTION('',(1.,0.,0.));
#6908=DIRECTION('',(0.,-4.44089209850063E-16,-1.));
#6909=DIRECTION('center_axis',(0.,2.41352831440251E-16,1.));
#6910=DIRECTION('ref_axis',(0.,-1.,2.41352831440251E-16));
#6911=DIRECTION('',(0.,-1.,2.41352831440251E-16));
#6912=DIRECTION('',(-1.,0.,0.));
#6913=DIRECTION('',(0.,1.,-2.41352831440251E-16));
#6914=DIRECTION('center_axis',(0.,-1.,2.41352831440251E-16));
#6915=DIRECTION('ref_axis',(0.,-2.41352831440251E-16,-1.));
#6916=DIRECTION('',(0.,-2.41352831440251E-16,-1.));
#6917=DIRECTION('',(1.,0.,0.));
#6918=DIRECTION('',(0.,2.41352831440251E-16,1.));
#6919=DIRECTION('',(1.,0.,0.));
#6920=DIRECTION('center_axis',(0.,0.,-1.));
#6921=DIRECTION('ref_axis',(0.,1.,0.));
#6922=DIRECTION('',(0.,1.,0.));
#6923=DIRECTION('',(1.,0.,0.));
#6924=DIRECTION('',(0.,-1.,0.));
#6925=DIRECTION('center_axis',(0.,-1.,0.));
#6926=DIRECTION('ref_axis',(0.,0.,-1.));
#6927=DIRECTION('',(0.,0.,-1.));
#6928=DIRECTION('',(1.,0.,0.));
#6929=DIRECTION('',(0.,0.,1.));
#6930=DIRECTION('center_axis',(0.,-0.707106781186547,0.707106781186548));
#6931=DIRECTION('ref_axis',(0.,-0.707106781186548,-0.707106781186547));
#6932=DIRECTION('',(0.,-0.707106781186548,-0.707106781186547));
#6933=DIRECTION('',(1.,0.,0.));
#6934=DIRECTION('',(0.,0.707106781186548,0.707106781186547));
#6935=DIRECTION('center_axis',(0.,0.,1.));
#6936=DIRECTION('ref_axis',(0.,-1.,0.));
#6937=DIRECTION('',(0.,-1.,0.));
#6938=DIRECTION('',(1.,0.,0.));
#6939=DIRECTION('',(0.,1.,0.));
#6940=DIRECTION('center_axis',(0.,0.707106781186548,0.707106781186547));
#6941=DIRECTION('ref_axis',(0.,-0.707106781186547,0.707106781186548));
#6942=DIRECTION('',(0.,-0.707106781186547,0.707106781186548));
#6943=DIRECTION('',(1.,0.,0.));
#6944=DIRECTION('',(0.,0.707106781186547,-0.707106781186548));
#6945=DIRECTION('center_axis',(0.,1.,0.));
#6946=DIRECTION('ref_axis',(0.,0.,1.));
#6947=DIRECTION('',(0.,0.,1.));
#6948=DIRECTION('',(1.,0.,0.));
#6949=DIRECTION('',(0.,0.,-1.));
#6950=DIRECTION('center_axis',(0.,0.,-1.));
#6951=DIRECTION('ref_axis',(0.,1.,0.));
#6952=DIRECTION('',(0.,1.,0.));
#6953=DIRECTION('',(1.,0.,0.));
#6954=DIRECTION('',(0.,-1.,0.));
#6955=DIRECTION('center_axis',(0.,1.,-2.41352831440251E-16));
#6956=DIRECTION('ref_axis',(0.,2.41352831440251E-16,1.));
#6957=DIRECTION('',(0.,2.41352831440251E-16,1.));
#6958=DIRECTION('',(-1.,0.,0.));
#6959=DIRECTION('',(0.,-2.41352831440251E-16,-1.));
#6960=DIRECTION('center_axis',(0.,0.,1.));
#6961=DIRECTION('ref_axis',(0.,-1.,0.));
#6962=DIRECTION('',(0.,-1.,0.));
#6963=DIRECTION('',(1.,0.,0.));
#6964=DIRECTION('',(0.,1.,0.));
#6965=DIRECTION('',(1.,0.,0.));
#6966=DIRECTION('center_axis',(0.,-1.,0.));
#6967=DIRECTION('ref_axis',(0.,0.,-1.));
#6968=DIRECTION('',(0.,0.,-1.));
#6969=DIRECTION('',(1.,0.,0.));
#6970=DIRECTION('',(0.,0.,1.));
#6971=DIRECTION('center_axis',(0.,0.,1.));
#6972=DIRECTION('ref_axis',(0.,-1.,0.));
#6973=DIRECTION('',(0.,-1.,0.));
#6974=DIRECTION('',(1.,0.,0.));
#6975=DIRECTION('',(0.,1.,0.));
#6976=DIRECTION('center_axis',(0.,0.707106781186548,0.707106781186548));
#6977=DIRECTION('ref_axis',(0.,-0.707106781186548,0.707106781186548));
#6978=DIRECTION('',(0.,-0.707106781186548,0.707106781186548));
#6979=DIRECTION('',(1.,0.,0.));
#6980=DIRECTION('',(0.,0.707106781186548,-0.707106781186548));
#6981=DIRECTION('center_axis',(0.,1.,0.));
#6982=DIRECTION('ref_axis',(0.,0.,1.));
#6983=DIRECTION('',(0.,0.,1.));
#6984=DIRECTION('',(1.,0.,0.));
#6985=DIRECTION('',(0.,0.,-1.));
#6986=DIRECTION('center_axis',(0.,0.707106781186548,-0.707106781186547));
#6987=DIRECTION('ref_axis',(0.,0.707106781186547,0.707106781186548));
#6988=DIRECTION('',(0.,0.707106781186547,0.707106781186548));
#6989=DIRECTION('',(1.,0.,0.));
#6990=DIRECTION('',(0.,-0.707106781186547,-0.707106781186548));
#6991=DIRECTION('center_axis',(0.,-7.40148683083438E-16,-1.));
#6992=DIRECTION('ref_axis',(0.,1.,-7.40148683083438E-16));
#6993=DIRECTION('',(0.,1.,-7.40148683083438E-16));
#6994=DIRECTION('',(1.,0.,0.));
#6995=DIRECTION('',(0.,-1.,7.40148683083438E-16));
#6996=DIRECTION('center_axis',(0.,-1.,0.));
#6997=DIRECTION('ref_axis',(0.,0.,-1.));
#6998=DIRECTION('',(0.,0.,-1.));
#6999=DIRECTION('',(1.,0.,0.));
#7000=DIRECTION('',(0.,0.,1.));
#7001=DIRECTION('center_axis',(0.,0.,-1.));
#7002=DIRECTION('ref_axis',(0.,1.,0.));
#7003=DIRECTION('',(0.,1.,0.));
#7004=DIRECTION('',(-1.,0.,0.));
#7005=DIRECTION('',(0.,-1.,0.));
#7006=DIRECTION('center_axis',(0.,1.,0.));
#7007=DIRECTION('ref_axis',(0.,0.,1.));
#7008=DIRECTION('',(0.,0.,1.));
#7009=DIRECTION('',(1.,0.,0.));
#7010=DIRECTION('',(0.,0.,-1.));
#7011=DIRECTION('',(1.,0.,0.));
#7012=DIRECTION('center_axis',(0.,0.,1.));
#7013=DIRECTION('ref_axis',(0.,-1.,0.));
#7014=DIRECTION('',(0.,-1.,0.));
#7015=DIRECTION('',(1.,0.,0.));
#7016=DIRECTION('',(0.,1.,0.));
#7017=DIRECTION('center_axis',(0.,1.,0.));
#7018=DIRECTION('ref_axis',(0.,0.,1.));
#7019=DIRECTION('',(0.,0.,1.));
#7020=DIRECTION('',(1.,0.,0.));
#7021=DIRECTION('',(0.,0.,-1.));
#7022=DIRECTION('center_axis',(0.,0.707106781186547,-0.707106781186548));
#7023=DIRECTION('ref_axis',(0.,0.707106781186548,0.707106781186547));
#7024=DIRECTION('',(0.,0.707106781186548,0.707106781186547));
#7025=DIRECTION('',(1.,0.,0.));
#7026=DIRECTION('',(0.,-0.707106781186548,-0.707106781186547));
#7027=DIRECTION('center_axis',(0.,0.,-1.));
#7028=DIRECTION('ref_axis',(0.,1.,0.));
#7029=DIRECTION('',(0.,1.,0.));
#7030=DIRECTION('',(1.,0.,0.));
#7031=DIRECTION('',(0.,-1.,0.));
#7032=DIRECTION('center_axis',(0.,-0.707106781186547,-0.707106781186548));
#7033=DIRECTION('ref_axis',(0.,0.707106781186548,-0.707106781186547));
#7034=DIRECTION('',(0.,0.707106781186548,-0.707106781186547));
#7035=DIRECTION('',(1.,0.,0.));
#7036=DIRECTION('',(0.,-0.707106781186548,0.707106781186547));
#7037=DIRECTION('center_axis',(0.,-1.,0.));
#7038=DIRECTION('ref_axis',(0.,0.,-1.));
#7039=DIRECTION('',(0.,0.,-1.));
#7040=DIRECTION('',(1.,0.,0.));
#7041=DIRECTION('',(0.,0.,1.));
#7042=DIRECTION('center_axis',(0.,0.,1.));
#7043=DIRECTION('ref_axis',(0.,-1.,0.));
#7044=DIRECTION('',(0.,-1.,0.));
#7045=DIRECTION('',(1.,0.,0.));
#7046=DIRECTION('',(0.,1.,0.));
#7047=DIRECTION('center_axis',(0.,-1.,0.));
#7048=DIRECTION('ref_axis',(0.,0.,-1.));
#7049=DIRECTION('',(0.,0.,-1.));
#7050=DIRECTION('',(-1.,0.,0.));
#7051=DIRECTION('',(0.,0.,1.));
#7052=DIRECTION('center_axis',(1.,0.,0.));
#7053=DIRECTION('ref_axis',(0.,0.,-1.));
#7054=DIRECTION('center_axis',(1.,0.,0.));
#7055=DIRECTION('ref_axis',(0.,0.,-1.));
#7056=DIRECTION('',(1.,0.,0.));
#7057=DIRECTION('center_axis',(-1.,0.,0.));
#7058=DIRECTION('ref_axis',(0.,0.,-1.));
#7059=DIRECTION('center_axis',(0.,1.,0.));
#7060=DIRECTION('ref_axis',(0.,0.,1.));
#7061=DIRECTION('',(0.,0.,1.));
#7062=DIRECTION('',(1.,0.,0.));
#7063=DIRECTION('',(0.,0.,1.));
#7064=DIRECTION('center_axis',(0.,1.,0.));
#7065=DIRECTION('ref_axis',(0.,0.,1.));
#7066=DIRECTION('',(0.,0.,1.));
#7067=DIRECTION('',(1.,0.,0.));
#7068=DIRECTION('',(0.,0.,1.));
#7069=DIRECTION('center_axis',(0.,0.,-1.));
#7070=DIRECTION('ref_axis',(0.,1.,0.));
#7071=DIRECTION('',(0.,1.,0.));
#7072=DIRECTION('',(0.,1.,0.));
#7073=DIRECTION('center_axis',(0.,0.,-1.));
#7074=DIRECTION('ref_axis',(0.,1.,0.));
#7075=DIRECTION('',(0.,1.,0.));
#7076=DIRECTION('',(1.,0.,0.));
#7077=DIRECTION('',(0.,1.,0.));
#7078=DIRECTION('center_axis',(0.,-1.,0.));
#7079=DIRECTION('ref_axis',(0.,0.,-1.));
#7080=DIRECTION('',(0.,0.,-1.));
#7081=DIRECTION('',(0.,0.,-1.));
#7082=DIRECTION('center_axis',(0.,-1.,0.));
#7083=DIRECTION('ref_axis',(0.,0.,-1.));
#7084=DIRECTION('',(0.,0.,-1.));
#7085=DIRECTION('',(1.,0.,0.));
#7086=DIRECTION('',(0.,0.,-1.));
#7087=DIRECTION('center_axis',(0.,0.,1.));
#7088=DIRECTION('ref_axis',(0.,-1.,0.));
#7089=DIRECTION('',(0.,-1.,0.));
#7090=DIRECTION('',(0.,-1.,0.));
#7091=DIRECTION('center_axis',(0.,0.,1.));
#7092=DIRECTION('ref_axis',(0.,-1.,0.));
#7093=DIRECTION('',(0.,-1.,0.));
#7094=DIRECTION('',(0.,-1.,0.));
#7095=DIRECTION('center_axis',(1.,0.,0.));
#7096=DIRECTION('ref_axis',(0.,0.,-1.));
#7097=DIRECTION('center_axis',(1.,0.,0.));
#7098=DIRECTION('ref_axis',(0.,0.,-1.));
#7099=DIRECTION('axis',(0.,0.,1.));
#7100=DIRECTION('refdir',(1.,0.,0.));
#7101=DIRECTION('center_axis',(0.,-0.707106781186548,-0.707106781186548));
#7102=DIRECTION('ref_axis',(-1.,0.,0.));
#7103=DIRECTION('',(0.,-0.707106781186548,0.707106781186548));
#7104=DIRECTION('',(-1.,0.,0.));
#7105=DIRECTION('',(0.,0.707106781186548,-0.707106781186548));
#7106=DIRECTION('',(1.,0.,0.));
#7107=DIRECTION('center_axis',(0.,0.707106781186548,0.707106781186548));
#7108=DIRECTION('ref_axis',(0.,0.707106781186547,-0.707106781186547));
#7109=DIRECTION('',(1.,0.,0.));
#7110=DIRECTION('center_axis',(0.,0.,1.));
#7111=DIRECTION('ref_axis',(1.,0.,0.));
#7112=DIRECTION('center_axis',(0.,0.,-1.));
#7113=DIRECTION('ref_axis',(1.,0.,0.));
#7114=DIRECTION('',(0.,0.,1.));
#7115=DIRECTION('center_axis',(0.,0.,-1.));
#7116=DIRECTION('ref_axis',(1.,0.,0.));
#7117=DIRECTION('center_axis',(0.,0.,-1.));
#7118=DIRECTION('ref_axis',(1.,0.,0.));
#7119=DIRECTION('center_axis',(0.,-0.707106781186548,0.707106781186548));
#7120=DIRECTION('ref_axis',(0.,0.707106781186547,0.707106781186547));
#7121=DIRECTION('center_axis',(0.,0.,-1.));
#7122=DIRECTION('ref_axis',(1.,0.,0.));
#7123=DIRECTION('center_axis',(0.,0.,1.));
#7124=DIRECTION('ref_axis',(1.,0.,0.));
#7125=DIRECTION('',(0.,-1.,0.));
#7126=DIRECTION('',(-1.,0.,0.));
#7127=DIRECTION('center_axis',(0.,0.,1.));
#7128=DIRECTION('ref_axis',(1.,0.,0.));
#7129=DIRECTION('',(-1.,0.,0.));
#7130=DIRECTION('',(0.,1.,0.));
#7131=DIRECTION('center_axis',(0.,0.707106781186548,-0.707106781186548));
#7132=DIRECTION('ref_axis',(-1.,0.,0.));
#7133=DIRECTION('',(0.,0.707106781186548,0.707106781186548));
#7134=DIRECTION('',(1.,0.,0.));
#7135=DIRECTION('',(0.,-0.707106781186548,-0.707106781186548));
#7136=DIRECTION('center_axis',(1.,0.,0.));
#7137=DIRECTION('ref_axis',(0.,1.,0.));
#7138=DIRECTION('',(0.,0.,1.));
#7139=DIRECTION('',(0.,1.,0.));
#7140=DIRECTION('',(0.,0.,1.));
#7141=DIRECTION('center_axis',(0.,1.,0.));
#7142=DIRECTION('ref_axis',(-1.,0.,0.));
#7143=DIRECTION('',(0.,0.,1.));
#7144=DIRECTION('',(-1.,0.,0.));
#7145=DIRECTION('center_axis',(0.,-1.,0.));
#7146=DIRECTION('ref_axis',(1.,0.,0.));
#7147=DIRECTION('',(1.,0.,0.));
#7148=DIRECTION('',(0.,0.,1.));
#7149=DIRECTION('center_axis',(-1.,0.,0.));
#7150=DIRECTION('ref_axis',(0.,-1.,0.));
#7151=DIRECTION('',(0.,-1.,0.));
#7152=DIRECTION('center_axis',(0.,0.,1.));
#7153=DIRECTION('ref_axis',(1.,0.,0.));
#7154=DIRECTION('axis',(0.,0.,1.));
#7155=DIRECTION('refdir',(1.,0.,0.));
#7156=DIRECTION('center_axis',(0.,1.,0.));
#7157=DIRECTION('ref_axis',(1.,0.,0.));
#7158=DIRECTION('center_axis',(0.,1.,0.));
#7159=DIRECTION('ref_axis',(1.,0.,0.));
#7160=DIRECTION('',(0.707106781186548,-0.707106781186547,-8.65956056235494E-17));
#7161=DIRECTION('center_axis',(0.,-1.,0.));
#7162=DIRECTION('ref_axis',(1.,0.,0.));
#7163=DIRECTION('center_axis',(0.,1.,0.));
#7164=DIRECTION('ref_axis',(1.,0.,0.));
#7165=DIRECTION('',(0.,-1.,0.));
#7166=DIRECTION('center_axis',(0.,-1.,0.));
#7167=DIRECTION('ref_axis',(1.,0.,0.));
#7168=DIRECTION('center_axis',(0.,1.,0.));
#7169=DIRECTION('ref_axis',(1.,0.,0.));
#7170=DIRECTION('center_axis',(0.,1.,0.));
#7171=DIRECTION('ref_axis',(1.,0.,0.));
#7172=DIRECTION('center_axis',(0.,1.,0.));
#7173=DIRECTION('ref_axis',(1.,0.,0.));
#7174=DIRECTION('',(0.,-1.,0.));
#7175=DIRECTION('center_axis',(0.,1.,0.));
#7176=DIRECTION('ref_axis',(1.,0.,0.));
#7177=DIRECTION('center_axis',(0.,1.,0.));
#7178=DIRECTION('ref_axis',(1.,0.,0.));
#7179=DIRECTION('axis',(0.,0.,1.));
#7180=DIRECTION('refdir',(1.,0.,0.));
#7181=DIRECTION('center_axis',(0.866025403784439,0.,-0.5));
#7182=DIRECTION('ref_axis',(0.5,0.,0.866025403784439));
#7183=DIRECTION('',(-0.5,0.,-0.866025403784439));
#7184=DIRECTION('',(0.,-1.,0.));
#7185=DIRECTION('',(0.5,0.,0.866025403784439));
#7186=DIRECTION('',(0.,-1.,0.));
#7187=DIRECTION('center_axis',(1.20185167898973E-16,0.,-1.));
#7188=DIRECTION('ref_axis',(1.,0.,1.20185167898973E-16));
#7189=DIRECTION('',(-1.,0.,-1.20185167898973E-16));
#7190=DIRECTION('',(0.,-1.,0.));
#7191=DIRECTION('',(1.,0.,1.20185167898973E-16));
#7192=DIRECTION('center_axis',(-0.866025403784439,0.,-0.5));
#7193=DIRECTION('ref_axis',(0.5,0.,-0.866025403784439));
#7194=DIRECTION('',(-0.5,0.,0.866025403784439));
#7195=DIRECTION('',(0.,-1.,0.));
#7196=DIRECTION('',(0.5,0.,-0.866025403784439));
#7197=DIRECTION('center_axis',(-0.866025403784439,0.,0.5));
#7198=DIRECTION('ref_axis',(-0.5,0.,-0.866025403784439));
#7199=DIRECTION('',(0.5,0.,0.866025403784439));
#7200=DIRECTION('',(0.,-1.,0.));
#7201=DIRECTION('',(-0.5,0.,-0.866025403784439));
#7202=DIRECTION('center_axis',(-2.40370335797945E-16,0.,1.));
#7203=DIRECTION('ref_axis',(-1.,0.,-2.40370335797945E-16));
#7204=DIRECTION('',(1.,0.,2.40370335797945E-16));
#7205=DIRECTION('',(0.,-1.,0.));
#7206=DIRECTION('',(-1.,0.,-2.40370335797945E-16));
#7207=DIRECTION('center_axis',(0.866025403784439,0.,0.5));
#7208=DIRECTION('ref_axis',(-0.5,0.,0.866025403784439));
#7209=DIRECTION('',(0.5,0.,-0.866025403784439));
#7210=DIRECTION('',(-0.5,0.,0.866025403784439));
#7211=DIRECTION('center_axis',(0.,1.,0.));
#7212=DIRECTION('ref_axis',(1.,0.,0.));
#7213=DIRECTION('center_axis',(0.,-1.,0.));
#7214=DIRECTION('ref_axis',(0.,0.,-1.));
#7215=DIRECTION('center_axis',(0.,1.,0.));
#7216=DIRECTION('ref_axis',(1.,0.,0.));
#7217=DIRECTION('center_axis',(0.,1.,0.));
#7218=DIRECTION('ref_axis',(1.,0.,0.));
#7219=DIRECTION('center_axis',(0.,1.,0.));
#7220=DIRECTION('ref_axis',(0.,0.,1.));
#7221=DIRECTION('center_axis',(0.,-1.,0.));
#7222=DIRECTION('ref_axis',(1.,0.,0.));
#7223=DIRECTION('center_axis',(0.,-1.,0.));
#7224=DIRECTION('ref_axis',(1.,0.,0.));
#7225=DIRECTION('center_axis',(0.,-1.,0.));
#7226=DIRECTION('ref_axis',(1.,0.,0.));
#7227=DIRECTION('',(0.707106781186548,0.707106781186547,8.65956056235493E-17));
#7228=DIRECTION('center_axis',(0.,-1.,0.));
#7229=DIRECTION('ref_axis',(1.,0.,0.));
#7230=DIRECTION('center_axis',(0.,-1.,0.));
#7231=DIRECTION('ref_axis',(1.,0.,0.));
#7232=DIRECTION('',(0.,1.,0.));
#7233=DIRECTION('center_axis',(0.,1.,0.));
#7234=DIRECTION('ref_axis',(1.,0.,0.));
#7235=DIRECTION('center_axis',(0.,-1.,0.));
#7236=DIRECTION('ref_axis',(1.,0.,0.));
#7237=DIRECTION('',(-0.707106781186547,0.707106781186548,-8.65956056235493E-17));
#7238=DIRECTION('center_axis',(0.,-1.,0.));
#7239=DIRECTION('ref_axis',(0.,0.,-1.));
#7240=DIRECTION('center_axis',(0.,-1.,0.));
#7241=DIRECTION('ref_axis',(1.,0.,0.));
#7242=DIRECTION('center_axis',(0.,1.,0.));
#7243=DIRECTION('ref_axis',(1.,0.,0.));
#7244=DIRECTION('center_axis',(0.,1.,0.));
#7245=DIRECTION('ref_axis',(1.,0.,0.));
#7246=DIRECTION('',(-0.447213595499958,0.894427190999916,-5.47678698264203E-17));
#7247=DIRECTION('center_axis',(0.,-1.,0.));
#7248=DIRECTION('ref_axis',(1.,0.,0.));
#7249=DIRECTION('',(0.,1.,0.));
#7250=DIRECTION('axis',(0.,0.,1.));
#7251=DIRECTION('refdir',(1.,0.,0.));
#7252=DIRECTION('center_axis',(0.,-1.,0.));
#7253=DIRECTION('ref_axis',(1.,0.,0.));
#7254=DIRECTION('center_axis',(0.,1.,0.));
#7255=DIRECTION('ref_axis',(1.,0.,0.));
#7256=DIRECTION('',(0.,1.,0.));
#7257=DIRECTION('center_axis',(0.,-1.,0.));
#7258=DIRECTION('ref_axis',(1.,0.,0.));
#7259=DIRECTION('center_axis',(0.,1.,0.));
#7260=DIRECTION('ref_axis',(1.,0.,0.));
#7261=DIRECTION('center_axis',(0.,-1.,0.));
#7262=DIRECTION('ref_axis',(1.,0.,0.));
#7263=DIRECTION('',(-0.707106781186549,0.707106781186546,-8.65956056235496E-17));
#7264=DIRECTION('center_axis',(0.,-1.,0.));
#7265=DIRECTION('ref_axis',(0.,0.,-1.));
#7266=DIRECTION('center_axis',(0.,-1.,0.));
#7267=DIRECTION('ref_axis',(1.,0.,0.));
#7268=DIRECTION('center_axis',(0.,1.,0.));
#7269=DIRECTION('ref_axis',(1.,0.,0.));
#7270=DIRECTION('',(-0.866025403784439,-0.5,-1.06057523872491E-16));
#7271=DIRECTION('center_axis',(1.4792020664489E-16,0.,-1.));
#7272=DIRECTION('ref_axis',(-1.,0.,-1.4792020664489E-16));
#7273=DIRECTION('',(0.,1.,0.));
#7274=DIRECTION('',(-1.,0.,-1.4792020664489E-16));
#7275=DIRECTION('',(0.,1.,0.));
#7276=DIRECTION('center_axis',(0.866025403784439,0.,-0.5));
#7277=DIRECTION('ref_axis',(-0.5,0.,-0.866025403784439));
#7278=DIRECTION('',(0.,1.,0.));
#7279=DIRECTION('',(-0.5,0.,-0.866025403784439));
#7280=DIRECTION('center_axis',(0.866025403784439,0.,0.5));
#7281=DIRECTION('ref_axis',(0.5,0.,-0.866025403784439));
#7282=DIRECTION('',(0.,1.,0.));
#7283=DIRECTION('',(0.5,0.,-0.866025403784439));
#7284=DIRECTION('center_axis',(-2.95840413289779E-16,0.,1.));
#7285=DIRECTION('ref_axis',(1.,0.,2.95840413289779E-16));
#7286=DIRECTION('',(0.,1.,0.));
#7287=DIRECTION('',(1.,0.,2.95840413289779E-16));
#7288=DIRECTION('center_axis',(-0.866025403784439,0.,0.5));
#7289=DIRECTION('ref_axis',(0.5,0.,0.866025403784439));
#7290=DIRECTION('',(0.,1.,0.));
#7291=DIRECTION('',(0.5,0.,0.866025403784439));
#7292=DIRECTION('center_axis',(-0.866025403784439,0.,-0.5));
#7293=DIRECTION('ref_axis',(-0.5,0.,0.866025403784439));
#7294=DIRECTION('',(-0.5,0.,0.866025403784439));
#7295=DIRECTION('center_axis',(0.,1.,0.));
#7296=DIRECTION('ref_axis',(0.,0.,1.));
#7297=DIRECTION('center_axis',(0.,1.,0.));
#7298=DIRECTION('ref_axis',(1.,0.,0.));
#7299=DIRECTION('axis',(0.,0.,1.));
#7300=DIRECTION('refdir',(1.,0.,0.));
#7301=DIRECTION('center_axis',(0.,1.,0.));
#7302=DIRECTION('ref_axis',(1.,0.,0.));
#7303=DIRECTION('',(0.866025403784439,-0.5,1.06057523872491E-16));
#7304=DIRECTION('center_axis',(0.,-1.,0.));
#7305=DIRECTION('ref_axis',(1.,0.,0.));
#7306=DIRECTION('center_axis',(0.,-1.,0.));
#7307=DIRECTION('ref_axis',(1.,0.,0.));
#7308=DIRECTION('center_axis',(0.,1.,0.));
#7309=DIRECTION('ref_axis',(1.,0.,0.));
#7310=DIRECTION('',(-0.866025403784439,-0.5,-1.06057523872491E-16));
#7311=DIRECTION('center_axis',(1.4792020664489E-16,0.,-1.));
#7312=DIRECTION('ref_axis',(-1.,0.,-1.4792020664489E-16));
#7313=DIRECTION('',(0.,1.,0.));
#7314=DIRECTION('',(0.,1.,0.));
#7315=DIRECTION('center_axis',(-0.866025403784439,0.,-0.5));
#7316=DIRECTION('ref_axis',(-0.5,0.,0.866025403784439));
#7317=DIRECTION('',(0.,1.,0.));
#7318=DIRECTION('center_axis',(-0.866025403784439,0.,0.5));
#7319=DIRECTION('ref_axis',(0.5,0.,0.866025403784439));
#7320=DIRECTION('',(0.,1.,0.));
#7321=DIRECTION('center_axis',(0.,1.,0.));
#7322=DIRECTION('ref_axis',(1.,0.,0.));
#7323=DIRECTION('center_axis',(0.,1.,0.));
#7324=DIRECTION('ref_axis',(1.,0.,0.));
#7325=DIRECTION('',(0.,-1.,0.));
#7326=DIRECTION('center_axis',(0.,1.,0.));
#7327=DIRECTION('ref_axis',(1.,0.,0.));
#7328=DIRECTION('center_axis',(-2.95840413289779E-16,0.,1.));
#7329=DIRECTION('ref_axis',(1.,0.,2.95840413289779E-16));
#7330=DIRECTION('',(0.,1.,0.));
#7331=DIRECTION('center_axis',(0.866025403784439,0.,-0.5));
#7332=DIRECTION('ref_axis',(-0.5,0.,-0.866025403784439));
#7333=DIRECTION('',(0.,1.,0.));
#7334=DIRECTION('center_axis',(0.866025403784439,0.,0.5));
#7335=DIRECTION('ref_axis',(0.5,0.,-0.866025403784439));
#7336=DIRECTION('center_axis',(0.,1.,0.));
#7337=DIRECTION('ref_axis',(1.,0.,0.));
#7338=DIRECTION('center_axis',(0.,1.,0.));
#7339=DIRECTION('ref_axis',(1.,0.,0.));
#7340=DIRECTION('axis',(0.,0.,1.));
#7341=DIRECTION('refdir',(1.,0.,0.));
#7342=DIRECTION('axis',(0.,0.,1.));
#7343=DIRECTION('refdir',(1.,0.,0.));
#7344=DIRECTION('center_axis',(0.,1.,0.));
#7345=DIRECTION('ref_axis',(1.,0.,0.));
#7346=DIRECTION('center_axis',(0.,1.,0.));
#7347=DIRECTION('ref_axis',(1.,0.,0.));
#7348=DIRECTION('',(0.,1.,0.));
#7349=DIRECTION('center_axis',(0.,-1.,0.));
#7350=DIRECTION('ref_axis',(1.,0.,0.));
#7351=DIRECTION('center_axis',(0.,1.,0.));
#7352=DIRECTION('ref_axis',(1.,0.,0.));
#7353=DIRECTION('center_axis',(0.,1.,0.));
#7354=DIRECTION('ref_axis',(1.,0.,0.));
#7355=DIRECTION('',(0.,1.,0.));
#7356=DIRECTION('center_axis',(0.,-1.,0.));
#7357=DIRECTION('ref_axis',(1.,0.,0.));
#7358=DIRECTION('center_axis',(0.,1.,0.));
#7359=DIRECTION('ref_axis',(1.,0.,0.));
#7360=DIRECTION('center_axis',(0.,1.,0.));
#7361=DIRECTION('ref_axis',(1.,0.,0.));
#7362=DIRECTION('',(0.,1.,0.));
#7363=DIRECTION('center_axis',(0.,-1.,0.));
#7364=DIRECTION('ref_axis',(1.,0.,0.));
#7365=DIRECTION('center_axis',(0.,1.,0.));
#7366=DIRECTION('ref_axis',(1.,0.,0.));
#7367=DIRECTION('center_axis',(0.,1.,0.));
#7368=DIRECTION('ref_axis',(1.,0.,0.));
#7369=DIRECTION('',(0.,1.,0.));
#7370=DIRECTION('center_axis',(0.,-1.,0.));
#7371=DIRECTION('ref_axis',(1.,0.,0.));
#7372=DIRECTION('center_axis',(0.,1.,0.));
#7373=DIRECTION('ref_axis',(1.,0.,0.));
#7374=DIRECTION('center_axis',(0.,-1.,0.));
#7375=DIRECTION('ref_axis',(1.,0.,0.));
#7376=DIRECTION('',(0.,-1.,0.));
#7377=DIRECTION('center_axis',(0.,-1.,0.));
#7378=DIRECTION('ref_axis',(1.,0.,0.));
#7379=DIRECTION('center_axis',(0.,1.,0.));
#7380=DIRECTION('ref_axis',(1.,0.,0.));
#7381=DIRECTION('center_axis',(0.,1.,0.));
#7382=DIRECTION('ref_axis',(1.,0.,0.));
#7383=DIRECTION('center_axis',(0.,1.,0.));
#7384=DIRECTION('ref_axis',(1.,0.,0.));
#7385=DIRECTION('',(0.,-1.,0.));
#7386=DIRECTION('center_axis',(0.,-1.,0.));
#7387=DIRECTION('ref_axis',(1.,0.,0.));
#7388=DIRECTION('center_axis',(0.,1.,0.));
#7389=DIRECTION('ref_axis',(1.,0.,0.));
#7390=DIRECTION('center_axis',(0.,1.,0.));
#7391=DIRECTION('ref_axis',(1.,0.,0.));
#7392=DIRECTION('',(0.,-1.,0.));
#7393=DIRECTION('center_axis',(0.,1.,0.));
#7394=DIRECTION('ref_axis',(1.,0.,0.));
#7395=DIRECTION('center_axis',(0.,1.,0.));
#7396=DIRECTION('ref_axis',(1.,0.,0.));
#7397=DIRECTION('center_axis',(0.,1.,0.));
#7398=DIRECTION('ref_axis',(1.,0.,0.));
#7399=DIRECTION('axis',(0.,0.,1.));
#7400=DIRECTION('refdir',(1.,0.,0.));
#7401=DIRECTION('center_axis',(0.,1.,0.));
#7402=DIRECTION('ref_axis',(1.,0.,0.));
#7403=DIRECTION('center_axis',(0.,1.,0.));
#7404=DIRECTION('ref_axis',(1.,0.,0.));
#7405=DIRECTION('',(0.,1.,0.));
#7406=DIRECTION('center_axis',(0.,-1.,0.));
#7407=DIRECTION('ref_axis',(1.,0.,0.));
#7408=DIRECTION('center_axis',(0.,1.,0.));
#7409=DIRECTION('ref_axis',(1.,0.,0.));
#7410=DIRECTION('center_axis',(0.,1.,0.));
#7411=DIRECTION('ref_axis',(1.,0.,0.));
#7412=DIRECTION('',(0.,1.,0.));
#7413=DIRECTION('center_axis',(0.,-1.,0.));
#7414=DIRECTION('ref_axis',(1.,0.,0.));
#7415=DIRECTION('center_axis',(0.,1.,0.));
#7416=DIRECTION('ref_axis',(1.,0.,0.));
#7417=DIRECTION('center_axis',(0.,1.,0.));
#7418=DIRECTION('ref_axis',(1.,0.,0.));
#7419=DIRECTION('',(0.,1.,0.));
#7420=DIRECTION('center_axis',(0.,-1.,0.));
#7421=DIRECTION('ref_axis',(1.,0.,0.));
#7422=DIRECTION('center_axis',(0.,1.,0.));
#7423=DIRECTION('ref_axis',(1.,0.,0.));
#7424=DIRECTION('center_axis',(0.,1.,0.));
#7425=DIRECTION('ref_axis',(1.,0.,0.));
#7426=DIRECTION('',(0.,1.,0.));
#7427=DIRECTION('center_axis',(0.,-1.,0.));
#7428=DIRECTION('ref_axis',(1.,0.,0.));
#7429=DIRECTION('center_axis',(0.,1.,0.));
#7430=DIRECTION('ref_axis',(1.,0.,0.));
#7431=DIRECTION('center_axis',(0.,-1.,0.));
#7432=DIRECTION('ref_axis',(1.,0.,0.));
#7433=DIRECTION('',(0.,-1.,0.));
#7434=DIRECTION('center_axis',(0.,-1.,0.));
#7435=DIRECTION('ref_axis',(1.,0.,0.));
#7436=DIRECTION('center_axis',(0.,1.,0.));
#7437=DIRECTION('ref_axis',(1.,0.,0.));
#7438=DIRECTION('center_axis',(0.,-1.,0.));
#7439=DIRECTION('ref_axis',(1.,0.,0.));
#7440=DIRECTION('center_axis',(0.,1.,0.));
#7441=DIRECTION('ref_axis',(1.,0.,0.));
#7442=DIRECTION('center_axis',(0.,-1.,0.));
#7443=DIRECTION('ref_axis',(1.,0.,0.));
#7444=DIRECTION('',(0.,-1.,0.));
#7445=DIRECTION('center_axis',(0.,1.,0.));
#7446=DIRECTION('ref_axis',(1.,0.,0.));
#7447=DIRECTION('center_axis',(0.,1.,0.));
#7448=DIRECTION('ref_axis',(1.,0.,0.));
#7449=DIRECTION('',(0.,-1.,0.));
#7450=DIRECTION('center_axis',(0.,1.,0.));
#7451=DIRECTION('ref_axis',(1.,0.,0.));
#7452=DIRECTION('center_axis',(0.,1.,0.));
#7453=DIRECTION('ref_axis',(1.,0.,0.));
#7454=DIRECTION('center_axis',(0.,1.,0.));
#7455=DIRECTION('ref_axis',(1.,0.,0.));
#7456=DIRECTION('axis',(0.,0.,1.));
#7457=DIRECTION('refdir',(1.,0.,0.));
#7458=DIRECTION('center_axis',(0.,1.,0.));
#7459=DIRECTION('ref_axis',(1.,0.,0.));
#7460=DIRECTION('center_axis',(0.,-1.,0.));
#7461=DIRECTION('ref_axis',(1.,0.,0.));
#7462=DIRECTION('',(0.,-1.,0.));
#7463=DIRECTION('center_axis',(0.,-1.,0.));
#7464=DIRECTION('ref_axis',(1.,0.,0.));
#7465=DIRECTION('center_axis',(0.,1.,0.));
#7466=DIRECTION('ref_axis',(1.,0.,0.));
#7467=DIRECTION('center_axis',(0.,1.,0.));
#7468=DIRECTION('ref_axis',(1.,0.,0.));
#7469=DIRECTION('',(0.,-1.,0.));
#7470=DIRECTION('center_axis',(0.,1.,0.));
#7471=DIRECTION('ref_axis',(1.,0.,0.));
#7472=DIRECTION('center_axis',(0.,1.,0.));
#7473=DIRECTION('ref_axis',(1.,0.,0.));
#7474=DIRECTION('center_axis',(0.,1.,0.));
#7475=DIRECTION('ref_axis',(1.,0.,0.));
#7476=DIRECTION('axis',(0.,0.,1.));
#7477=DIRECTION('refdir',(1.,0.,0.));
#7478=DIRECTION('center_axis',(0.,1.,0.));
#7479=DIRECTION('ref_axis',(1.,0.,0.));
#7480=DIRECTION('center_axis',(0.,1.,0.));
#7481=DIRECTION('ref_axis',(1.,0.,0.));
#7482=DIRECTION('',(0.,1.,0.));
#7483=DIRECTION('center_axis',(0.,-1.,0.));
#7484=DIRECTION('ref_axis',(1.,0.,0.));
#7485=DIRECTION('center_axis',(0.,1.,0.));
#7486=DIRECTION('ref_axis',(1.,0.,0.));
#7487=DIRECTION('center_axis',(0.,1.,0.));
#7488=DIRECTION('ref_axis',(1.,0.,0.));
#7489=DIRECTION('',(0.,1.,0.));
#7490=DIRECTION('center_axis',(0.,-1.,0.));
#7491=DIRECTION('ref_axis',(1.,0.,0.));
#7492=DIRECTION('center_axis',(0.,1.,0.));
#7493=DIRECTION('ref_axis',(1.,0.,0.));
#7494=DIRECTION('center_axis',(0.,1.,0.));
#7495=DIRECTION('ref_axis',(1.,0.,0.));
#7496=DIRECTION('',(0.,1.,0.));
#7497=DIRECTION('center_axis',(0.,-1.,0.));
#7498=DIRECTION('ref_axis',(1.,0.,0.));
#7499=DIRECTION('center_axis',(0.,1.,0.));
#7500=DIRECTION('ref_axis',(1.,0.,0.));
#7501=DIRECTION('center_axis',(0.,1.,0.));
#7502=DIRECTION('ref_axis',(1.,0.,0.));
#7503=DIRECTION('',(0.,1.,0.));
#7504=DIRECTION('center_axis',(0.,-1.,0.));
#7505=DIRECTION('ref_axis',(1.,0.,0.));
#7506=DIRECTION('center_axis',(0.,1.,0.));
#7507=DIRECTION('ref_axis',(1.,0.,0.));
#7508=DIRECTION('center_axis',(0.,-1.,0.));
#7509=DIRECTION('ref_axis',(1.,0.,0.));
#7510=DIRECTION('',(0.,-1.,0.));
#7511=DIRECTION('center_axis',(0.,-1.,0.));
#7512=DIRECTION('ref_axis',(1.,0.,0.));
#7513=DIRECTION('center_axis',(0.,1.,0.));
#7514=DIRECTION('ref_axis',(1.,0.,0.));
#7515=DIRECTION('center_axis',(0.,1.,0.));
#7516=DIRECTION('ref_axis',(1.,0.,0.));
#7517=DIRECTION('',(0.,-1.,0.));
#7518=DIRECTION('center_axis',(0.,1.,0.));
#7519=DIRECTION('ref_axis',(1.,0.,0.));
#7520=DIRECTION('center_axis',(0.,1.,0.));
#7521=DIRECTION('ref_axis',(1.,0.,0.));
#7522=DIRECTION('center_axis',(0.,1.,0.));
#7523=DIRECTION('ref_axis',(1.,0.,0.));
#7524=DIRECTION('axis',(0.,0.,1.));
#7525=DIRECTION('refdir',(1.,0.,0.));
#7526=DIRECTION('center_axis',(0.,1.,0.));
#7527=DIRECTION('ref_axis',(0.,0.,1.));
#7528=DIRECTION('center_axis',(0.,-1.,0.));
#7529=DIRECTION('ref_axis',(1.,0.,0.));
#7530=DIRECTION('center_axis',(0.,-1.,0.));
#7531=DIRECTION('ref_axis',(1.,0.,0.));
#7532=DIRECTION('center_axis',(0.,-1.,0.));
#7533=DIRECTION('ref_axis',(1.,0.,0.));
#7534=DIRECTION('',(0.707106781186547,0.707106781186548,8.65956056235493E-17));
#7535=DIRECTION('center_axis',(0.,-1.,0.));
#7536=DIRECTION('ref_axis',(1.,0.,0.));
#7537=DIRECTION('center_axis',(0.,-1.,0.));
#7538=DIRECTION('ref_axis',(1.,0.,0.));
#7539=DIRECTION('',(0.,1.,0.));
#7540=DIRECTION('center_axis',(0.,1.,0.));
#7541=DIRECTION('ref_axis',(1.,0.,0.));
#7542=DIRECTION('center_axis',(0.,-1.,0.));
#7543=DIRECTION('ref_axis',(1.,0.,0.));
#7544=DIRECTION('',(-0.707106781186547,0.707106781186548,-8.65956056235493E-17));
#7545=DIRECTION('center_axis',(0.,-1.,0.));
#7546=DIRECTION('ref_axis',(0.,0.,-1.));
#7547=DIRECTION('center_axis',(0.,-1.,0.));
#7548=DIRECTION('ref_axis',(1.,0.,0.));
#7549=DIRECTION('center_axis',(0.,1.,0.));
#7550=DIRECTION('ref_axis',(1.,0.,0.));
#7551=DIRECTION('center_axis',(0.,1.,0.));
#7552=DIRECTION('ref_axis',(1.,0.,0.));
#7553=DIRECTION('',(-0.447213595499958,0.894427190999916,-5.47678698264203E-17));
#7554=DIRECTION('center_axis',(0.,-1.,0.));
#7555=DIRECTION('ref_axis',(1.,0.,0.));
#7556=DIRECTION('center_axis',(0.,1.,0.));
#7557=DIRECTION('ref_axis',(1.,0.,0.));
#7558=DIRECTION('',(0.,1.,0.));
#7559=DIRECTION('center_axis',(0.,1.,0.));
#7560=DIRECTION('ref_axis',(1.,0.,0.));
#7561=DIRECTION('center_axis',(0.,-1.,0.));
#7562=DIRECTION('ref_axis',(1.,0.,0.));
#7563=DIRECTION('',(-0.707106781186547,0.707106781186548,-8.65956056235493E-17));
#7564=DIRECTION('center_axis',(0.,-1.,0.));
#7565=DIRECTION('ref_axis',(0.,0.,-1.));
#7566=DIRECTION('center_axis',(0.866025403784439,0.,-0.5));
#7567=DIRECTION('ref_axis',(0.5,0.,0.866025403784439));
#7568=DIRECTION('',(-0.5,0.,-0.866025403784439));
#7569=DIRECTION('',(0.,-1.,0.));
#7570=DIRECTION('',(0.5,0.,0.866025403784439));
#7571=DIRECTION('',(0.,-1.,0.));
#7572=DIRECTION('center_axis',(1.60246890531964E-16,0.,-1.));
#7573=DIRECTION('ref_axis',(1.,0.,1.60246890531964E-16));
#7574=DIRECTION('',(-1.,0.,-1.60246890531964E-16));
#7575=DIRECTION('',(0.,-1.,0.));
#7576=DIRECTION('',(1.,0.,1.60246890531964E-16));
#7577=DIRECTION('center_axis',(-0.866025403784439,0.,-0.5));
#7578=DIRECTION('ref_axis',(0.5,0.,-0.866025403784439));
#7579=DIRECTION('',(-0.5,0.,0.866025403784439));
#7580=DIRECTION('',(0.,-1.,0.));
#7581=DIRECTION('',(0.5,0.,-0.866025403784439));
#7582=DIRECTION('center_axis',(-0.866025403784439,0.,0.5));
#7583=DIRECTION('ref_axis',(-0.5,0.,-0.866025403784439));
#7584=DIRECTION('',(0.5,0.,0.866025403784439));
#7585=DIRECTION('',(0.,-1.,0.));
#7586=DIRECTION('',(-0.5,0.,-0.866025403784439));
#7587=DIRECTION('center_axis',(-1.60246890531964E-16,0.,1.));
#7588=DIRECTION('ref_axis',(-1.,0.,-1.60246890531964E-16));
#7589=DIRECTION('',(1.,0.,1.60246890531964E-16));
#7590=DIRECTION('',(0.,-1.,0.));
#7591=DIRECTION('',(-1.,0.,-1.60246890531964E-16));
#7592=DIRECTION('center_axis',(0.866025403784439,0.,0.5));
#7593=DIRECTION('ref_axis',(-0.5,0.,0.866025403784439));
#7594=DIRECTION('',(0.5,0.,-0.866025403784439));
#7595=DIRECTION('',(-0.5,0.,0.866025403784439));
#7596=DIRECTION('center_axis',(0.,1.,0.));
#7597=DIRECTION('ref_axis',(1.,0.,0.));
#7598=DIRECTION('center_axis',(0.,-1.,0.));
#7599=DIRECTION('ref_axis',(0.,0.,-1.));
#7600=DIRECTION('',(0.,0.,1.));
#7601=DIRECTION('',(1.,0.,0.));
#7602=DIRECTION('',(0.,0.,1.));
#7603=DIRECTION('',(1.,0.,0.));
#7604=DIRECTION('',(0.,0.,1.));
#7605=DIRECTION('',(1.,0.,0.));
#7606=DIRECTION('',(0.,0.,1.));
#7607=DIRECTION('',(1.,0.,0.));
#7608=DIRECTION('',(0.,0.,1.));
#7609=DIRECTION('',(1.,0.,0.));
#7610=DIRECTION('',(0.,0.,1.));
#7611=DIRECTION('',(-1.,1.22464679914735E-16,0.));
#7612=DIRECTION('',(0.,0.,1.));
#7613=DIRECTION('',(1.,0.,0.));
#7614=DIRECTION('',(0.,0.,1.));
#7615=DIRECTION('',(1.,0.,0.));
#7616=DIRECTION('',(0.,0.,1.));
#7617=DIRECTION('',(1.,0.,0.));
#7618=DIRECTION('',(0.,0.,1.));
#7619=DIRECTION('',(1.,0.,0.));
#7620=DIRECTION('',(0.,0.,1.));
#7621=DIRECTION('',(1.,0.,0.));
#7622=DIRECTION('',(0.,0.,1.));
#7623=DIRECTION('',(1.,0.,0.));
#7624=DIRECTION('',(0.,0.,1.));
#7625=DIRECTION('',(1.,0.,0.));
#7626=DIRECTION('',(0.,0.,1.));
#7627=DIRECTION('',(1.,0.,0.));
#7628=DIRECTION('',(0.,0.,1.));
#7629=DIRECTION('',(1.,0.,0.));
#7630=DIRECTION('',(0.,0.,1.));
#7631=DIRECTION('',(1.,0.,0.));
#7632=DIRECTION('',(0.,0.,1.));
#7633=DIRECTION('',(1.,0.,0.));
#7634=DIRECTION('',(0.,-1.,2.22044604925031E-16));
#7635=DIRECTION('',(1.,0.,0.));
#7636=DIRECTION('',(0.,-1.,2.22044604925031E-16));
#7637=DIRECTION('',(1.,0.,0.));
#7638=DIRECTION('',(0.,0.,1.));
#7639=DIRECTION('',(1.,0.,0.));
#7640=DIRECTION('',(0.,-1.,2.22044604925031E-16));
#7641=DIRECTION('',(1.,0.,0.));
#7642=DIRECTION('',(0.,-1.,2.22044604925031E-16));
#7643=DIRECTION('',(1.,0.,0.));
#7644=DIRECTION('',(0.,0.,1.));
#7645=DIRECTION('',(1.,0.,0.));
#7646=DIRECTION('',(0.,-1.,2.22044604925031E-16));
#7647=DIRECTION('',(1.,0.,0.));
#7648=DIRECTION('',(0.,-1.,2.22044604925031E-16));
#7649=DIRECTION('',(1.,0.,0.));
#7650=DIRECTION('',(0.,0.,1.));
#7651=DIRECTION('',(2.22044604925031E-16,1.,0.));
#7652=DIRECTION('',(0.,0.,1.));
#7653=DIRECTION('',(2.22044604925031E-16,-1.,0.));
#7654=DIRECTION('',(0.,0.,1.));
#7655=DIRECTION('',(1.,0.,0.));
#7656=DIRECTION('',(0.,0.,1.));
#7657=DIRECTION('',(1.,0.,0.));
#7658=DIRECTION('',(0.,-1.,2.22044604925031E-16));
#7659=DIRECTION('',(1.,0.,0.));
#7660=DIRECTION('',(0.,-1.,2.22044604925031E-16));
#7661=DIRECTION('',(1.,0.,0.));
#7662=DIRECTION('',(0.,0.,1.));
#7663=DIRECTION('',(1.,0.,0.));
#7664=DIRECTION('',(0.,-1.,2.22044604925031E-16));
#7665=DIRECTION('',(1.,0.,0.));
#7666=DIRECTION('',(0.,-1.,2.22044604925031E-16));
#7667=DIRECTION('',(1.,0.,0.));
#7668=DIRECTION('',(0.,0.,1.));
#7669=DIRECTION('',(1.,0.,0.));
#7670=DIRECTION('',(0.,-1.,2.22044604925031E-16));
#7671=DIRECTION('',(1.,0.,0.));
#7672=DIRECTION('',(0.,-1.,2.22044604925031E-16));
#7673=DIRECTION('',(1.,0.,0.));
#7674=DIRECTION('',(0.,0.,1.));
#7675=DIRECTION('',(2.22044604925031E-16,1.,0.));
#7676=DIRECTION('',(0.,0.,1.));
#7677=DIRECTION('',(2.22044604925031E-16,-1.,0.));
#7678=DIRECTION('',(0.,0.,1.));
#7679=DIRECTION('',(1.,0.,0.));
#7680=DIRECTION('',(0.,0.,1.));
#7681=DIRECTION('',(1.,0.,0.));
#7682=DIRECTION('',(0.,0.,1.));
#7683=DIRECTION('',(1.,0.,0.));
#7684=DIRECTION('',(0.,0.,1.));
#7685=DIRECTION('',(1.,0.,0.));
#7686=DIRECTION('',(0.,0.,1.));
#7687=DIRECTION('',(-1.,1.22464679914735E-16,0.));
#7688=DIRECTION('',(0.,0.,1.));
#7689=DIRECTION('',(-1.,1.22464679914735E-16,0.));
#7690=DIRECTION('',(0.,0.,1.));
#7691=DIRECTION('',(-1.,1.22464679914735E-16,0.));
#7692=DIRECTION('',(0.,0.,1.));
#7693=DIRECTION('',(-1.,1.22464679914735E-16,0.));
#7694=DIRECTION('',(0.,0.,1.));
#7695=DIRECTION('',(1.,0.,0.));
#7696=DIRECTION('',(0.,0.,1.));
#7697=DIRECTION('',(1.,0.,0.));
#7698=DIRECTION('',(0.,0.,1.));
#7699=DIRECTION('',(1.,0.,0.));
#7700=DIRECTION('',(0.,0.,1.));
#7701=DIRECTION('',(1.,0.,0.));
#7702=DIRECTION('',(0.,0.,1.));
#7703=DIRECTION('',(1.,0.,0.));
#7704=DIRECTION('',(0.,0.,1.));
#7705=DIRECTION('',(1.,0.,0.));
#7706=DIRECTION('',(0.,0.,1.));
#7707=DIRECTION('',(1.,0.,0.));
#7708=CARTESIAN_POINT('',(0.,0.,0.));
#7709=CARTESIAN_POINT('',(0.,0.,0.));
#7710=CARTESIAN_POINT('',(0.,0.,0.));
#7711=CARTESIAN_POINT('Origin',(0.,30.8,4.5));
#7712=CARTESIAN_POINT('',(-0.165,30.8,4.5));
#7713=CARTESIAN_POINT('Origin',(0.,30.8,4.5));
#7714=CARTESIAN_POINT('',(-0.165,32.5,4.5));
#7715=CARTESIAN_POINT('',(-0.165,30.8,4.5));
#7716=CARTESIAN_POINT('Origin',(0.,32.5,4.5));
#7717=CARTESIAN_POINT('Origin',(0.,30.8,4.5));
#7718=CARTESIAN_POINT('Origin',(0.,-2.6,4.5));
#7719=CARTESIAN_POINT('',(-0.165,-2.5,4.5));
#7720=CARTESIAN_POINT('Origin',(0.,-2.5,4.5));
#7721=CARTESIAN_POINT('',(-0.165,-0.8,4.5));
#7722=CARTESIAN_POINT('',(-0.165,-2.6,4.5));
#7723=CARTESIAN_POINT('Origin',(0.,-0.8,4.5));
#7724=CARTESIAN_POINT('Origin',(0.,-0.8,4.5));
#7725=CARTESIAN_POINT('Origin',(0.,29.1,4.5));
#7726=CARTESIAN_POINT('',(-0.6,29.1,4.5));
#7727=CARTESIAN_POINT('Origin',(0.,29.1,4.5));
#7728=CARTESIAN_POINT('',(-0.5,29.1,4.5));
#7729=CARTESIAN_POINT('Origin',(0.,29.1,4.5));
#7730=CARTESIAN_POINT('Origin',(0.,0.9,4.5));
#7731=CARTESIAN_POINT('',(-0.6,0.9,4.5));
#7732=CARTESIAN_POINT('Origin',(0.,0.9,4.5));
#7733=CARTESIAN_POINT('',(-0.5,0.9,4.5));
#7734=CARTESIAN_POINT('Origin',(0.,0.9,4.5));
#7735=CARTESIAN_POINT('Origin',(0.,0.9,4.5));
#7736=CARTESIAN_POINT('',(-0.6,0.9,4.5));
#7737=CARTESIAN_POINT('Origin',(0.,-2.5,4.5));
#7738=CARTESIAN_POINT('',(-0.5,-2.5,4.5));
#7739=CARTESIAN_POINT('',(-0.5,-2.5,4.5));
#7740=CARTESIAN_POINT('Origin',(0.,-2.5,4.5));
#7741=CARTESIAN_POINT('Origin',(0.,-2.5,4.5));
#7742=CARTESIAN_POINT('',(-0.5,32.5,4.5));
#7743=CARTESIAN_POINT('Origin',(0.,32.5,4.5));
#7744=CARTESIAN_POINT('',(-0.5,-2.5,4.5));
#7745=CARTESIAN_POINT('Origin',(0.,32.5,4.5));
#7746=CARTESIAN_POINT('Origin',(0.,-2.5,4.5));
#7747=CARTESIAN_POINT('',(0.,0.,0.));
#7748=CARTESIAN_POINT('Origin',(0.,-1.6,4.5));
#7749=CARTESIAN_POINT('',(-0.505,0.,4.5));
#7750=CARTESIAN_POINT('Origin',(0.,0.,4.5));
#7751=CARTESIAN_POINT('',(-0.505,-1.6,4.5));
#7752=CARTESIAN_POINT('',(-0.505,-1.6,4.5));
#7753=CARTESIAN_POINT('Origin',(0.,-1.6,4.5));
#7754=CARTESIAN_POINT('Origin',(0.,-1.6,4.5));
#7755=CARTESIAN_POINT('',(-0.8,0.,4.5));
#7756=CARTESIAN_POINT('Origin',(0.,0.,4.5));
#7757=CARTESIAN_POINT('',(-0.8,-1.6,4.5));
#7758=CARTESIAN_POINT('',(-0.8,-1.6,4.5));
#7759=CARTESIAN_POINT('Origin',(0.,-1.6,4.5));
#7760=CARTESIAN_POINT('Origin',(0.,0.,4.5));
#7761=CARTESIAN_POINT('Origin',(0.,-1.6,4.5));
#7762=CARTESIAN_POINT('',(0.,0.,0.));
#7763=CARTESIAN_POINT('Origin',(0.,30.,4.5));
#7764=CARTESIAN_POINT('',(-0.505,31.6,4.5));
#7765=CARTESIAN_POINT('Origin',(0.,31.6,4.5));
#7766=CARTESIAN_POINT('',(-0.505,30.,4.5));
#7767=CARTESIAN_POINT('',(-0.505,30.,4.5));
#7768=CARTESIAN_POINT('Origin',(0.,30.,4.5));
#7769=CARTESIAN_POINT('Origin',(0.,30.,4.5));
#7770=CARTESIAN_POINT('',(-0.8,31.6,4.5));
#7771=CARTESIAN_POINT('Origin',(0.,31.6,4.5));
#7772=CARTESIAN_POINT('',(-0.8,30.,4.5));
#7773=CARTESIAN_POINT('',(-0.8,30.,4.5));
#7774=CARTESIAN_POINT('Origin',(0.,30.,4.5));
#7775=CARTESIAN_POINT('Origin',(0.,31.6,4.5));
#7776=CARTESIAN_POINT('Origin',(0.,30.,4.5));
#7777=CARTESIAN_POINT('',(0.,0.,0.));
#7778=CARTESIAN_POINT('Origin',(0.,-2.8,4.5));
#7779=CARTESIAN_POINT('',(-0.225,-2.5,4.5));
#7780=CARTESIAN_POINT('Origin',(0.,-2.5,4.5));
#7781=CARTESIAN_POINT('',(-0.225,-2.8,4.5));
#7782=CARTESIAN_POINT('',(-0.225,-2.8,4.5));
#7783=CARTESIAN_POINT('Origin',(0.,-2.8,4.5));
#7784=CARTESIAN_POINT('Origin',(0.,-2.8,4.5));
#7785=CARTESIAN_POINT('',(-1.1,-2.5,4.5));
#7786=CARTESIAN_POINT('Origin',(0.,-2.5,4.5));
#7787=CARTESIAN_POINT('',(-1.1,-2.8,4.5));
#7788=CARTESIAN_POINT('',(-1.1,-2.8,4.5));
#7789=CARTESIAN_POINT('Origin',(0.,-2.8,4.5));
#7790=CARTESIAN_POINT('Origin',(0.,-2.5,4.5));
#7791=CARTESIAN_POINT('Origin',(0.,-2.8,4.5));
#7792=CARTESIAN_POINT('',(0.,0.,0.));
#7793=CARTESIAN_POINT('Origin',(0.,-2.5,4.5));
#7794=CARTESIAN_POINT('',(-0.605,-2.4,4.5));
#7795=CARTESIAN_POINT('Origin',(0.,-2.4,4.5));
#7796=CARTESIAN_POINT('',(-0.605,-2.5,4.5));
#7797=CARTESIAN_POINT('',(-0.605,-2.5,4.5));
#7798=CARTESIAN_POINT('Origin',(0.,-2.5,4.5));
#7799=CARTESIAN_POINT('Origin',(0.,-2.5,4.5));
#7800=CARTESIAN_POINT('',(-1.,-2.4,4.5));
#7801=CARTESIAN_POINT('Origin',(0.,-2.4,4.5));
#7802=CARTESIAN_POINT('',(-1.,-2.5,4.5));
#7803=CARTESIAN_POINT('',(-1.,-2.5,4.5));
#7804=CARTESIAN_POINT('Origin',(0.,-2.5,4.5));
#7805=CARTESIAN_POINT('Origin',(0.,-2.4,4.5));
#7806=CARTESIAN_POINT('Origin',(0.,-2.5,4.5));
#7807=CARTESIAN_POINT('',(0.,0.,0.));
#7808=CARTESIAN_POINT('',(0.,0.,0.));
#7809=CARTESIAN_POINT('Origin',(0.,0.,0.));
#7810=CARTESIAN_POINT('',(-0.976185,-0.246528389340863,-1.19548183562566E-16));
#7811=CARTESIAN_POINT('',(-1.19548183562566E-16,-0.246528389340863,0.976185));
#7812=CARTESIAN_POINT('Origin',(0.,-0.246528389340863,0.));
#7813=CARTESIAN_POINT('Origin',(0.,-0.246528389340863,0.));
#7814=CARTESIAN_POINT('',(-1.19548183562566E-16,0.246528389340863,0.976185));
#7815=CARTESIAN_POINT('Origin',(-1.22464679914735E-16,0.,1.));
#7816=CARTESIAN_POINT('',(-0.976185,0.246528389340863,1.19548183562566E-16));
#7817=CARTESIAN_POINT('Origin',(0.,0.246528389340863,0.));
#7818=CARTESIAN_POINT('Origin',(0.,0.246528389340863,0.));
#7819=CARTESIAN_POINT('Origin',(0.,0.,0.));
#7820=CARTESIAN_POINT('',(-0.976185,0.45,-1.19548183562566E-16));
#7821=CARTESIAN_POINT('',(-0.976185,0.,-1.19548183562566E-16));
#7822=CARTESIAN_POINT('Origin',(0.,0.45,0.));
#7823=CARTESIAN_POINT('Origin',(0.,0.,0.));
#7824=CARTESIAN_POINT('',(-0.5,-0.39,-6.12323399573677E-17));
#7825=CARTESIAN_POINT('Origin',(0.,-0.39,0.));
#7826=CARTESIAN_POINT('',(-0.5,0.39,-6.12323399573677E-17));
#7827=CARTESIAN_POINT('',(-0.5,0.,-6.12323399573677E-17));
#7828=CARTESIAN_POINT('Origin',(0.,0.39,0.));
#7829=CARTESIAN_POINT('Origin',(0.,0.42,0.));
#7830=CARTESIAN_POINT('',(-0.56,0.45,-6.85802207522518E-17));
#7831=CARTESIAN_POINT('',(-0.53,0.42,-6.49062803548097E-17));
#7832=CARTESIAN_POINT('Origin',(0.,0.45,0.));
#7833=CARTESIAN_POINT('Origin',(0.976185,0.45,0.));
#7834=CARTESIAN_POINT('Origin',(0.,0.,0.));
#7835=CARTESIAN_POINT('',(-0.976185,-0.45,-1.19548183562566E-16));
#7836=CARTESIAN_POINT('Origin',(0.,-0.45,0.));
#7837=CARTESIAN_POINT('',(-0.976185,0.,-1.19548183562566E-16));
#7838=CARTESIAN_POINT('Origin',(0.56,-0.45,0.));
#7839=CARTESIAN_POINT('',(-0.56,-0.45,-6.85802207522518E-17));
#7840=CARTESIAN_POINT('Origin',(0.,-0.45,0.));
#7841=CARTESIAN_POINT('Origin',(0.,-0.42,0.));
#7842=CARTESIAN_POINT('',(-0.53,-0.42,-6.49062803548097E-17));
#7843=CARTESIAN_POINT('',(0.,0.,0.));
#7844=CARTESIAN_POINT('Origin',(0.,0.,0.));
#7845=CARTESIAN_POINT('',(-1.023815,0.246528389340863,-1.25381176266905E-16));
#7846=CARTESIAN_POINT('',(-1.25381176266905E-16,0.246528389340863,1.023815));
#7847=CARTESIAN_POINT('Origin',(0.,0.246528389340863,0.));
#7848=CARTESIAN_POINT('Origin',(0.,0.246528389340863,0.));
#7849=CARTESIAN_POINT('',(-1.25381176266905E-16,-0.246528389340863,1.023815));
#7850=CARTESIAN_POINT('Origin',(-1.22464679914735E-16,0.,1.));
#7851=CARTESIAN_POINT('',(-1.023815,-0.246528389340863,1.25381176266905E-16));
#7852=CARTESIAN_POINT('Origin',(0.,-0.246528389340863,0.));
#7853=CARTESIAN_POINT('Origin',(0.,-0.246528389340863,0.));
#7854=CARTESIAN_POINT('Origin',(0.,0.,0.));
#7855=CARTESIAN_POINT('',(-1.023815,-0.45,-1.25381176266905E-16));
#7856=CARTESIAN_POINT('Origin',(0.,-0.45,0.));
#7857=CARTESIAN_POINT('',(-1.023815,0.,-1.25381176266905E-16));
#7858=CARTESIAN_POINT('Origin',(1.44,0.45,0.));
#7859=CARTESIAN_POINT('',(-1.44,0.45,-1.76349139077219E-16));
#7860=CARTESIAN_POINT('Origin',(0.,0.45,0.));
#7861=CARTESIAN_POINT('',(-1.023815,0.45,-1.25381176266905E-16));
#7862=CARTESIAN_POINT('Origin',(0.,0.45,0.));
#7863=CARTESIAN_POINT('Origin',(0.,0.42,0.));
#7864=CARTESIAN_POINT('',(-1.5,0.39,-1.83697019872103E-16));
#7865=CARTESIAN_POINT('Origin',(0.,0.39,0.));
#7866=CARTESIAN_POINT('',(-1.47,0.42,-1.80023079474661E-16));
#7867=CARTESIAN_POINT('Origin',(0.,0.,0.));
#7868=CARTESIAN_POINT('',(-1.5,-0.39,-1.83697019872103E-16));
#7869=CARTESIAN_POINT('Origin',(0.,-0.39,0.));
#7870=CARTESIAN_POINT('',(-1.5,0.,-1.83697019872103E-16));
#7871=CARTESIAN_POINT('Origin',(0.,-0.42,0.));
#7872=CARTESIAN_POINT('',(-1.44,-0.45,-1.76349139077219E-16));
#7873=CARTESIAN_POINT('Origin',(0.,-0.45,0.));
#7874=CARTESIAN_POINT('',(-1.47,-0.42,-1.80023079474661E-16));
#7875=CARTESIAN_POINT('Origin',(1.023815,-0.45,0.));
#7876=CARTESIAN_POINT('Origin',(0.,0.,0.));
#7877=CARTESIAN_POINT('',(-1.023815,0.,-1.25381176266905E-16));
#7878=CARTESIAN_POINT('',(0.,0.,0.));
#7879=CARTESIAN_POINT('Origin',(1.,0.,0.));
#7880=CARTESIAN_POINT('',(1.,-1.78583896120461E-33,0.23815));
#7881=CARTESIAN_POINT('',(1.,-1.78583896120461E-33,-0.23815));
#7882=CARTESIAN_POINT('Origin',(1.,0.,0.));
#7883=CARTESIAN_POINT('Origin',(0.707106781186548,0.,-0.707106781186547));
#7884=CARTESIAN_POINT('',(0.875504261126124,-1.78583896120461E-33,-0.538709301246971));
#7885=CARTESIAN_POINT('',(0.538709301246971,-1.78583896120461E-33,-0.875504261126124));
#7886=CARTESIAN_POINT('Origin',(0.707106781186548,0.,-0.707106781186547));
#7887=CARTESIAN_POINT('Origin',(6.12323399573677E-17,0.,-1.));
#7888=CARTESIAN_POINT('',(0.23815,-1.78583896120461E-33,-1.));
#7889=CARTESIAN_POINT('',(-0.23815,-1.78583896120461E-33,-1.));
#7890=CARTESIAN_POINT('Origin',(6.12323399573677E-17,0.,-1.));
#7891=CARTESIAN_POINT('Origin',(-0.707106781186547,0.,-0.707106781186548));
#7892=CARTESIAN_POINT('',(-0.538709301246971,-1.78583896120461E-33,-0.875504261126124));
#7893=CARTESIAN_POINT('',(-0.875504261126124,-1.78583896120461E-33,-0.538709301246971));
#7894=CARTESIAN_POINT('Origin',(-0.707106781186547,0.,-0.707106781186548));
#7895=CARTESIAN_POINT('Origin',(-1.,0.,-1.22464679914735E-16));
#7896=CARTESIAN_POINT('',(-1.,-1.78583896120461E-33,-0.23815));
#7897=CARTESIAN_POINT('',(-1.,-1.78583896120461E-33,0.23815));
#7898=CARTESIAN_POINT('Origin',(-1.,0.,-1.22464679914735E-16));
#7899=CARTESIAN_POINT('Origin',(-0.707106781186548,0.,0.707106781186547));
#7900=CARTESIAN_POINT('',(-0.875504261126124,-7.94881478324376E-33,0.538709301246971));
#7901=CARTESIAN_POINT('',(-0.538709301246971,4.37713686083455E-33,0.875504261126124));
#7902=CARTESIAN_POINT('Origin',(-0.707106781186548,0.,0.707106781186547));
#7903=CARTESIAN_POINT('Origin',(-1.83697019872103E-16,0.,1.));
#7904=CARTESIAN_POINT('',(-0.23815,-1.78583896120461E-33,1.));
#7905=CARTESIAN_POINT('',(0.23815,-1.78583896120461E-33,1.));
#7906=CARTESIAN_POINT('Origin',(-1.83697019872103E-16,0.,1.));
#7907=CARTESIAN_POINT('Origin',(0.707106781186547,0.,0.707106781186548));
#7908=CARTESIAN_POINT('',(0.538709301246971,-4.86732687222419E-33,0.875504261126124));
#7909=CARTESIAN_POINT('',(0.875504261126124,1.29564894981497E-33,0.538709301246971));
#7910=CARTESIAN_POINT('Origin',(0.707106781186547,0.,0.707106781186548));
#7911=CARTESIAN_POINT('',(0.,0.,0.));
#7912=CARTESIAN_POINT('Origin',(0.707106781186547,0.,0.707106781186548));
#7913=CARTESIAN_POINT('',(0.504455939115715,-0.04763,0.841298510752802));
#7914=CARTESIAN_POINT('',(0.841298510752802,-0.04763,0.504455939115715));
#7915=CARTESIAN_POINT('Ctrl Pts',(0.504455939115715,-0.04763,0.841298510752802));
#7916=CARTESIAN_POINT('Ctrl Pts',(0.508899795931835,-0.0740444353928835,
0.838633903678357));
#7917=CARTESIAN_POINT('Ctrl Pts',(0.517157748491652,-0.0999305678883309,
0.833661031856294));
#7918=CARTESIAN_POINT('Ctrl Pts',(0.537715343527944,-0.142345102874864,
0.820511285096538));
#7919=CARTESIAN_POINT('Ctrl Pts',(0.548874290046456,-0.159766064500479,
0.813159949759));
#7920=CARTESIAN_POINT('Ctrl Pts',(0.573915184558107,-0.190326085855194,
0.795684265985089));
#7921=CARTESIAN_POINT('Ctrl Pts',(0.587792702767295,-0.203463743702801,
0.78555112003688));
#7922=CARTESIAN_POINT('Ctrl Pts',(0.615966552324775,-0.224161999508995,
0.763642258217233));
#7923=CARTESIAN_POINT('Ctrl Pts',(0.631684198665438,-0.232861760990032,
0.750785745543687));
#7924=CARTESIAN_POINT('Ctrl Pts',(0.663382628119203,-0.244251601209411,
0.722929908501543));
#7925=CARTESIAN_POINT('Ctrl Pts',(0.679352081686668,-0.246942143572133,
0.707917883896095));
#7926=CARTESIAN_POINT('Ctrl Pts',(0.707917883896095,-0.246942143572133,
0.679352081686668));
#7927=CARTESIAN_POINT('Ctrl Pts',(0.722929908501543,-0.244251601209411,
0.663382628119203));
#7928=CARTESIAN_POINT('Ctrl Pts',(0.750785745543687,-0.232861760990032,
0.631684198665439));
#7929=CARTESIAN_POINT('Ctrl Pts',(0.763642258217232,-0.224161999508995,
0.615966552324775));
#7930=CARTESIAN_POINT('Ctrl Pts',(0.78555112003688,-0.203463743702801,0.587792702767295));
#7931=CARTESIAN_POINT('Ctrl Pts',(0.795684265985088,-0.190326085855194,
0.573915184558108));
#7932=CARTESIAN_POINT('Ctrl Pts',(0.813159949759,-0.15976606450048,0.548874290046456));
#7933=CARTESIAN_POINT('Ctrl Pts',(0.820511285096538,-0.142345102874864,
0.537715343527944));
#7934=CARTESIAN_POINT('Ctrl Pts',(0.833661031856294,-0.099930567888331,
0.517157748491653));
#7935=CARTESIAN_POINT('Ctrl Pts',(0.838633903678357,-0.0740444353928835,
0.508899795931835));
#7936=CARTESIAN_POINT('Ctrl Pts',(0.841298510752801,-0.0476299999999999,
0.504455939115715));
#7937=CARTESIAN_POINT('',(0.528110872004958,-0.04763,0.871530771444223));
#7938=CARTESIAN_POINT('Origin',(0.707106781186547,-0.04763,0.707106781186548));
#7939=CARTESIAN_POINT('',(0.871530771444223,-0.04763,0.528110872004959));
#7940=CARTESIAN_POINT('Ctrl Pts',(0.871530771444223,-0.0476300000000001,
0.528110872004958));
#7941=CARTESIAN_POINT('Ctrl Pts',(0.87014664509073,-0.0609922781173483,
0.530395067942936));
#7942=CARTESIAN_POINT('Ctrl Pts',(0.868149331745851,-0.0742967091364493,
0.533674141594226));
#7943=CARTESIAN_POINT('Ctrl Pts',(0.85981294420286,-0.115492077056649,0.54708917182331));
#7944=CARTESIAN_POINT('Ctrl Pts',(0.850993704737257,-0.141695629206859,
0.560922177770136));
#7945=CARTESIAN_POINT('Ctrl Pts',(0.830754510485543,-0.181890537957859,
0.590422647829571));
#7946=CARTESIAN_POINT('Ctrl Pts',(0.816896541396381,-0.201072148666545,
0.609616703125488));
#7947=CARTESIAN_POINT('Ctrl Pts',(0.792310597819928,-0.223955109275652,
0.641117951819998));
#7948=CARTESIAN_POINT('Ctrl Pts',(0.779109323683612,-0.232742381310829,
0.657208095763053));
#7949=CARTESIAN_POINT('Ctrl Pts',(0.750552691816206,-0.244234834628584,
0.68964083160521));
#7950=CARTESIAN_POINT('Ctrl Pts',(0.735185187071673,-0.246942143572133,
0.705971972091755));
#7951=CARTESIAN_POINT('Ctrl Pts',(0.705971972091754,-0.246942143572133,
0.735185187071673));
#7952=CARTESIAN_POINT('Ctrl Pts',(0.689640831605209,-0.244234834628584,
0.750552691816206));
#7953=CARTESIAN_POINT('Ctrl Pts',(0.657208095763052,-0.232742381310829,
0.779109323683612));
#7954=CARTESIAN_POINT('Ctrl Pts',(0.641117951819998,-0.223955109275652,
0.792310597819928));
#7955=CARTESIAN_POINT('Ctrl Pts',(0.609616703125487,-0.201072148666545,
0.816896541396382));
#7956=CARTESIAN_POINT('Ctrl Pts',(0.590422647829571,-0.181890537957858,
0.830754510485544));
#7957=CARTESIAN_POINT('Ctrl Pts',(0.560922177770135,-0.141695629206858,
0.850993704737257));
#7958=CARTESIAN_POINT('Ctrl Pts',(0.547089171823309,-0.115492077056649,
0.859812944202861));
#7959=CARTESIAN_POINT('Ctrl Pts',(0.533674141594226,-0.0742967091364491,
0.868149331745852));
#7960=CARTESIAN_POINT('Ctrl Pts',(0.530395067942936,-0.0609922781173483,
0.870146645090731));
#7961=CARTESIAN_POINT('Ctrl Pts',(0.528110872004958,-0.0476300000000001,
0.871530771444223));
#7962=CARTESIAN_POINT('Origin',(0.707106781186547,-0.04763,0.707106781186548));
#7963=CARTESIAN_POINT('Origin',(0.,-0.166705,0.));
#7964=CARTESIAN_POINT('',(0.242834539687906,-0.04763,0.989696097314));
#7965=CARTESIAN_POINT('Origin',(0.,-0.04763,0.));
#7966=CARTESIAN_POINT('',(-0.242834539687907,-0.04763,0.989696097314));
#7967=CARTESIAN_POINT('Ctrl Pts',(0.242834539687906,-0.04763,0.989696097314));
#7968=CARTESIAN_POINT('Ctrl Pts',(0.24024064412003,-0.0609922781173483,
0.990332542620729));
#7969=CARTESIAN_POINT('Ctrl Pts',(0.236509675094874,-0.0742967091364492,
0.991238884025248));
#7970=CARTESIAN_POINT('Ctrl Pts',(0.221129100087819,-0.115492077056649,
0.994830026707808));
#7971=CARTESIAN_POINT('Ctrl Pts',(0.205111543747588,-0.141695629206859,
0.998375294985966));
#7972=CARTESIAN_POINT('Ctrl Pts',(0.169940289819232,-0.181890537957859,
1.00492400591205));
#7973=CARTESIAN_POINT('Ctrl Pts',(0.1465689792446,-0.201072148666545,1.00869718865384));
#7974=CARTESIAN_POINT('Ctrl Pts',(0.106909345252087,-0.223955109275652,
1.01358704779679));
#7975=CARTESIAN_POINT('Ctrl Pts',(0.0861971848975941,-0.232742381310829,
1.0156297872271));
#7976=CARTESIAN_POINT('Ctrl Pts',(0.0430711894098822,-0.244234834628584,
1.01837060663223));
#7977=CARTESIAN_POINT('Ctrl Pts',(0.0206568624125605,-0.246942143572133,
1.019052));
#7978=CARTESIAN_POINT('Ctrl Pts',(-0.0206568624125608,-0.246942143572133,
1.019052));
#7979=CARTESIAN_POINT('Ctrl Pts',(-0.0430711894098825,-0.244234834628584,
1.01837060663223));
#7980=CARTESIAN_POINT('Ctrl Pts',(-0.0861971848975943,-0.232742381310829,
1.0156297872271));
#7981=CARTESIAN_POINT('Ctrl Pts',(-0.106909345252088,-0.223955109275652,
1.01358704779679));
#7982=CARTESIAN_POINT('Ctrl Pts',(-0.1465689792446,-0.201072148666545,1.00869718865384));
#7983=CARTESIAN_POINT('Ctrl Pts',(-0.169940289819232,-0.181890537957859,
1.00492400591205));
#7984=CARTESIAN_POINT('Ctrl Pts',(-0.205111543747588,-0.141695629206859,
0.998375294985966));
#7985=CARTESIAN_POINT('Ctrl Pts',(-0.221129100087819,-0.115492077056649,
0.994830026707808));
#7986=CARTESIAN_POINT('Ctrl Pts',(-0.236509675094875,-0.0742967091364493,
0.991238884025248));
#7987=CARTESIAN_POINT('Ctrl Pts',(-0.24024064412003,-0.0609922781173483,
0.990332542620729));
#7988=CARTESIAN_POINT('Ctrl Pts',(-0.242834539687907,-0.04763,0.989696097314));
#7989=CARTESIAN_POINT('',(-0.528110872004959,-0.04763,0.871530771444223));
#7990=CARTESIAN_POINT('Origin',(0.,-0.04763,0.));
#7991=CARTESIAN_POINT('',(-0.871530771444223,-0.04763,0.528110872004958));
#7992=CARTESIAN_POINT('Ctrl Pts',(-0.528110872004958,-0.0476300000000001,
0.871530771444223));
#7993=CARTESIAN_POINT('Ctrl Pts',(-0.530395067942936,-0.0609922781173484,
0.87014664509073));
#7994=CARTESIAN_POINT('Ctrl Pts',(-0.533674141594226,-0.0742967091364493,
0.868149331745851));
#7995=CARTESIAN_POINT('Ctrl Pts',(-0.54708917182331,-0.115492077056649,
0.85981294420286));
#7996=CARTESIAN_POINT('Ctrl Pts',(-0.560922177770136,-0.141695629206859,
0.850993704737257));
#7997=CARTESIAN_POINT('Ctrl Pts',(-0.590422647829571,-0.181890537957859,
0.830754510485543));
#7998=CARTESIAN_POINT('Ctrl Pts',(-0.609616703125488,-0.201072148666545,
0.816896541396381));
#7999=CARTESIAN_POINT('Ctrl Pts',(-0.641117951819998,-0.223955109275652,
0.792310597819928));
#8000=CARTESIAN_POINT('Ctrl Pts',(-0.657208095763053,-0.232742381310829,
0.779109323683611));
#8001=CARTESIAN_POINT('Ctrl Pts',(-0.68964083160521,-0.244234834628584,
0.750552691816205));
#8002=CARTESIAN_POINT('Ctrl Pts',(-0.705971972091755,-0.246942143572133,
0.735185187071673));
#8003=CARTESIAN_POINT('Ctrl Pts',(-0.735185187071673,-0.246942143572133,
0.705971972091754));
#8004=CARTESIAN_POINT('Ctrl Pts',(-0.750552691816206,-0.244234834628584,
0.689640831605209));
#8005=CARTESIAN_POINT('Ctrl Pts',(-0.779109323683612,-0.232742381310829,
0.657208095763052));
#8006=CARTESIAN_POINT('Ctrl Pts',(-0.792310597819928,-0.223955109275652,
0.641117951819998));
#8007=CARTESIAN_POINT('Ctrl Pts',(-0.816896541396382,-0.201072148666545,
0.609616703125487));
#8008=CARTESIAN_POINT('Ctrl Pts',(-0.830754510485544,-0.181890537957858,
0.590422647829571));
#8009=CARTESIAN_POINT('Ctrl Pts',(-0.850993704737257,-0.141695629206858,
0.560922177770135));
#8010=CARTESIAN_POINT('Ctrl Pts',(-0.859812944202861,-0.115492077056649,
0.547089171823309));
#8011=CARTESIAN_POINT('Ctrl Pts',(-0.868149331745852,-0.0742967091364491,
0.533674141594226));
#8012=CARTESIAN_POINT('Ctrl Pts',(-0.870146645090731,-0.0609922781173483,
0.530395067942936));
#8013=CARTESIAN_POINT('Ctrl Pts',(-0.871530771444223,-0.04763,0.528110872004958));
#8014=CARTESIAN_POINT('',(-0.989696097314,-0.04763,0.242834539687906));
#8015=CARTESIAN_POINT('Origin',(0.,-0.04763,0.));
#8016=CARTESIAN_POINT('',(-1.019052,-0.246942143572133,1.248489836334E-16));
#8017=CARTESIAN_POINT('Ctrl Pts',(-0.989696097314,-0.04763,0.242834539687906));
#8018=CARTESIAN_POINT('Ctrl Pts',(-0.990332542620729,-0.0609922781173483,
0.24024064412003));
#8019=CARTESIAN_POINT('Ctrl Pts',(-0.991238884025248,-0.0742967091364492,
0.236509675094874));
#8020=CARTESIAN_POINT('Ctrl Pts',(-0.994830026707808,-0.115492077056649,
0.221129100087819));
#8021=CARTESIAN_POINT('Ctrl Pts',(-0.998375294985966,-0.141695629206859,
0.205111543747588));
#8022=CARTESIAN_POINT('Ctrl Pts',(-1.00492400591205,-0.181890537957859,
0.169940289819232));
#8023=CARTESIAN_POINT('Ctrl Pts',(-1.00869718865384,-0.201072148666545,
0.1465689792446));
#8024=CARTESIAN_POINT('Ctrl Pts',(-1.01358704779679,-0.223955109275652,
0.106909345252088));
#8025=CARTESIAN_POINT('Ctrl Pts',(-1.0156297872271,-0.232742381310829,0.0861971848975944));
#8026=CARTESIAN_POINT('Ctrl Pts',(-1.01837060663223,-0.244234834628584,
0.0430711894098825));
#8027=CARTESIAN_POINT('Ctrl Pts',(-1.019052,-0.246942143572133,0.0206568624125608));
#8028=CARTESIAN_POINT('Ctrl Pts',(-1.019052,-0.246942143572133,1.2490009027033E-16));
#8029=CARTESIAN_POINT('',(-1.019052,-0.28578,1.24797876996471E-16));
#8030=CARTESIAN_POINT('',(-1.019052,-0.166705,1.24797876996471E-16));
#8031=CARTESIAN_POINT('Origin',(0.,-0.28578,0.));
#8032=CARTESIAN_POINT('',(-0.989696097314,-0.04763,-0.242834539687906));
#8033=CARTESIAN_POINT('Ctrl Pts',(-1.019052,-0.246942143572133,1.2490009027033E-16));
#8034=CARTESIAN_POINT('Ctrl Pts',(-1.019052,-0.246942143572133,-0.0206568624125605));
#8035=CARTESIAN_POINT('Ctrl Pts',(-1.01837060663223,-0.244234834628584,
-0.0430711894098822));
#8036=CARTESIAN_POINT('Ctrl Pts',(-1.0156297872271,-0.232742381310829,-0.0861971848975941));
#8037=CARTESIAN_POINT('Ctrl Pts',(-1.01358704779679,-0.223955109275652,
-0.106909345252087));
#8038=CARTESIAN_POINT('Ctrl Pts',(-1.00869718865384,-0.201072148666546,
-0.1465689792446));
#8039=CARTESIAN_POINT('Ctrl Pts',(-1.00492400591205,-0.181890537957859,
-0.169940289819232));
#8040=CARTESIAN_POINT('Ctrl Pts',(-0.998375294985966,-0.141695629206859,
-0.205111543747588));
#8041=CARTESIAN_POINT('Ctrl Pts',(-0.994830026707808,-0.11549207705665,
-0.221129100087819));
#8042=CARTESIAN_POINT('Ctrl Pts',(-0.991238884025248,-0.0742967091364495,
-0.236509675094874));
#8043=CARTESIAN_POINT('Ctrl Pts',(-0.990332542620729,-0.0609922781173484,
-0.24024064412003));
#8044=CARTESIAN_POINT('Ctrl Pts',(-0.989696097314,-0.0476300000000001,-0.242834539687907));
#8045=CARTESIAN_POINT('',(-0.871530771444223,-0.04763,-0.528110872004958));
#8046=CARTESIAN_POINT('Origin',(0.,-0.04763,0.));
#8047=CARTESIAN_POINT('',(-0.528110872004958,-0.04763,-0.871530771444223));
#8048=CARTESIAN_POINT('Ctrl Pts',(-0.871530771444223,-0.0476300000000001,
-0.528110872004958));
#8049=CARTESIAN_POINT('Ctrl Pts',(-0.87014664509073,-0.0609922781173484,
-0.530395067942936));
#8050=CARTESIAN_POINT('Ctrl Pts',(-0.868149331745851,-0.0742967091364494,
-0.533674141594226));
#8051=CARTESIAN_POINT('Ctrl Pts',(-0.85981294420286,-0.115492077056649,
-0.54708917182331));
#8052=CARTESIAN_POINT('Ctrl Pts',(-0.850993704737257,-0.141695629206859,
-0.560922177770136));
#8053=CARTESIAN_POINT('Ctrl Pts',(-0.830754510485543,-0.181890537957859,
-0.590422647829571));
#8054=CARTESIAN_POINT('Ctrl Pts',(-0.816896541396381,-0.201072148666546,
-0.609616703125488));
#8055=CARTESIAN_POINT('Ctrl Pts',(-0.792310597819928,-0.223955109275652,
-0.641117951819999));
#8056=CARTESIAN_POINT('Ctrl Pts',(-0.779109323683611,-0.232742381310829,
-0.657208095763053));
#8057=CARTESIAN_POINT('Ctrl Pts',(-0.750552691816205,-0.244234834628584,
-0.68964083160521));
#8058=CARTESIAN_POINT('Ctrl Pts',(-0.735185187071673,-0.246942143572133,
-0.705971972091755));
#8059=CARTESIAN_POINT('Ctrl Pts',(-0.705971972091754,-0.246942143572133,
-0.735185187071673));
#8060=CARTESIAN_POINT('Ctrl Pts',(-0.68964083160521,-0.244234834628584,
-0.750552691816206));
#8061=CARTESIAN_POINT('Ctrl Pts',(-0.657208095763052,-0.232742381310829,
-0.779109323683612));
#8062=CARTESIAN_POINT('Ctrl Pts',(-0.641117951819998,-0.223955109275652,
-0.792310597819928));
#8063=CARTESIAN_POINT('Ctrl Pts',(-0.609616703125488,-0.201072148666545,
-0.816896541396381));
#8064=CARTESIAN_POINT('Ctrl Pts',(-0.590422647829571,-0.181890537957859,
-0.830754510485543));
#8065=CARTESIAN_POINT('Ctrl Pts',(-0.560922177770136,-0.141695629206859,
-0.850993704737257));
#8066=CARTESIAN_POINT('Ctrl Pts',(-0.54708917182331,-0.115492077056649,
-0.85981294420286));
#8067=CARTESIAN_POINT('Ctrl Pts',(-0.533674141594226,-0.0742967091364494,
-0.868149331745852));
#8068=CARTESIAN_POINT('Ctrl Pts',(-0.530395067942936,-0.0609922781173484,
-0.870146645090731));
#8069=CARTESIAN_POINT('Ctrl Pts',(-0.528110872004958,-0.0476300000000001,
-0.871530771444223));
#8070=CARTESIAN_POINT('',(-0.242834539687906,-0.04763,-0.989696097314));
#8071=CARTESIAN_POINT('Origin',(0.,-0.04763,0.));
#8072=CARTESIAN_POINT('',(0.242834539687906,-0.04763,-0.989696097314));
#8073=CARTESIAN_POINT('Ctrl Pts',(-0.242834539687907,-0.04763,-0.989696097314));
#8074=CARTESIAN_POINT('Ctrl Pts',(-0.24024064412003,-0.0609922781173483,
-0.990332542620729));
#8075=CARTESIAN_POINT('Ctrl Pts',(-0.236509675094874,-0.0742967091364493,
-0.991238884025248));
#8076=CARTESIAN_POINT('Ctrl Pts',(-0.221129100087819,-0.115492077056649,
-0.994830026707808));
#8077=CARTESIAN_POINT('Ctrl Pts',(-0.205111543747588,-0.141695629206859,
-0.998375294985966));
#8078=CARTESIAN_POINT('Ctrl Pts',(-0.169940289819232,-0.181890537957859,
-1.00492400591205));
#8079=CARTESIAN_POINT('Ctrl Pts',(-0.1465689792446,-0.201072148666545,-1.00869718865384));
#8080=CARTESIAN_POINT('Ctrl Pts',(-0.106909345252087,-0.223955109275652,
-1.01358704779679));
#8081=CARTESIAN_POINT('Ctrl Pts',(-0.0861971848975942,-0.232742381310829,
-1.0156297872271));
#8082=CARTESIAN_POINT('Ctrl Pts',(-0.0430711894098823,-0.244234834628584,
-1.01837060663223));
#8083=CARTESIAN_POINT('Ctrl Pts',(-0.0206568624125606,-0.246942143572133,
-1.019052));
#8084=CARTESIAN_POINT('Ctrl Pts',(0.0206568624125607,-0.246942143572133,
-1.019052));
#8085=CARTESIAN_POINT('Ctrl Pts',(0.0430711894098824,-0.244234834628584,
-1.01837060663223));
#8086=CARTESIAN_POINT('Ctrl Pts',(0.0861971848975943,-0.232742381310829,
-1.0156297872271));
#8087=CARTESIAN_POINT('Ctrl Pts',(0.106909345252088,-0.223955109275652,
-1.01358704779679));
#8088=CARTESIAN_POINT('Ctrl Pts',(0.1465689792446,-0.201072148666545,-1.00869718865384));
#8089=CARTESIAN_POINT('Ctrl Pts',(0.169940289819232,-0.181890537957859,
-1.00492400591205));
#8090=CARTESIAN_POINT('Ctrl Pts',(0.205111543747588,-0.141695629206859,
-0.998375294985966));
#8091=CARTESIAN_POINT('Ctrl Pts',(0.221129100087819,-0.115492077056649,
-0.994830026707808));
#8092=CARTESIAN_POINT('Ctrl Pts',(0.236509675094874,-0.0742967091364493,
-0.991238884025248));
#8093=CARTESIAN_POINT('Ctrl Pts',(0.24024064412003,-0.0609922781173484,
-0.990332542620729));
#8094=CARTESIAN_POINT('Ctrl Pts',(0.242834539687907,-0.04763,-0.989696097314));
#8095=CARTESIAN_POINT('',(0.528110872004958,-0.04763,-0.871530771444223));
#8096=CARTESIAN_POINT('Origin',(0.,-0.04763,0.));
#8097=CARTESIAN_POINT('',(0.871530771444223,-0.04763,-0.528110872004958));
#8098=CARTESIAN_POINT('Ctrl Pts',(0.528110872004958,-0.0476300000000001,
-0.871530771444223));
#8099=CARTESIAN_POINT('Ctrl Pts',(0.530395067942936,-0.0609922781173484,
-0.870146645090731));
#8100=CARTESIAN_POINT('Ctrl Pts',(0.533674141594226,-0.0742967091364493,
-0.868149331745851));
#8101=CARTESIAN_POINT('Ctrl Pts',(0.54708917182331,-0.115492077056649,-0.85981294420286));
#8102=CARTESIAN_POINT('Ctrl Pts',(0.560922177770136,-0.141695629206859,
-0.850993704737257));
#8103=CARTESIAN_POINT('Ctrl Pts',(0.590422647829571,-0.181890537957859,
-0.830754510485543));
#8104=CARTESIAN_POINT('Ctrl Pts',(0.609616703125488,-0.201072148666545,
-0.816896541396381));
#8105=CARTESIAN_POINT('Ctrl Pts',(0.641117951819998,-0.223955109275652,
-0.792310597819928));
#8106=CARTESIAN_POINT('Ctrl Pts',(0.657208095763053,-0.232742381310829,
-0.779109323683612));
#8107=CARTESIAN_POINT('Ctrl Pts',(0.68964083160521,-0.244234834628584,-0.750552691816206));
#8108=CARTESIAN_POINT('Ctrl Pts',(0.705971972091755,-0.246942143572133,
-0.735185187071673));
#8109=CARTESIAN_POINT('Ctrl Pts',(0.735185187071673,-0.246942143572133,
-0.705971972091754));
#8110=CARTESIAN_POINT('Ctrl Pts',(0.750552691816206,-0.244234834628584,
-0.68964083160521));
#8111=CARTESIAN_POINT('Ctrl Pts',(0.779109323683612,-0.232742381310829,
-0.657208095763053));
#8112=CARTESIAN_POINT('Ctrl Pts',(0.792310597819928,-0.223955109275652,
-0.641117951819998));
#8113=CARTESIAN_POINT('Ctrl Pts',(0.816896541396381,-0.201072148666545,
-0.609616703125488));
#8114=CARTESIAN_POINT('Ctrl Pts',(0.830754510485543,-0.181890537957859,
-0.590422647829571));
#8115=CARTESIAN_POINT('Ctrl Pts',(0.850993704737257,-0.141695629206859,
-0.560922177770136));
#8116=CARTESIAN_POINT('Ctrl Pts',(0.85981294420286,-0.115492077056649,-0.54708917182331));
#8117=CARTESIAN_POINT('Ctrl Pts',(0.868149331745851,-0.0742967091364493,
-0.533674141594226));
#8118=CARTESIAN_POINT('Ctrl Pts',(0.870146645090731,-0.0609922781173484,
-0.530395067942936));
#8119=CARTESIAN_POINT('Ctrl Pts',(0.871530771444223,-0.0476300000000001,
-0.528110872004958));
#8120=CARTESIAN_POINT('',(0.989696097314,-0.04763,-0.242834539687906));
#8121=CARTESIAN_POINT('Origin',(0.,-0.04763,0.));
#8122=CARTESIAN_POINT('',(0.989696097314,-0.04763,0.242834539687906));
#8123=CARTESIAN_POINT('Ctrl Pts',(0.989696097314,-0.04763,-0.242834539687907));
#8124=CARTESIAN_POINT('Ctrl Pts',(0.990332542620729,-0.0609922781173483,
-0.24024064412003));
#8125=CARTESIAN_POINT('Ctrl Pts',(0.991238884025248,-0.0742967091364493,
-0.236509675094874));
#8126=CARTESIAN_POINT('Ctrl Pts',(0.994830026707808,-0.115492077056649,
-0.221129100087819));
#8127=CARTESIAN_POINT('Ctrl Pts',(0.998375294985966,-0.141695629206859,
-0.205111543747588));
#8128=CARTESIAN_POINT('Ctrl Pts',(1.00492400591205,-0.181890537957859,-0.169940289819232));
#8129=CARTESIAN_POINT('Ctrl Pts',(1.00869718865384,-0.201072148666545,-0.1465689792446));
#8130=CARTESIAN_POINT('Ctrl Pts',(1.01358704779679,-0.223955109275652,-0.106909345252087));
#8131=CARTESIAN_POINT('Ctrl Pts',(1.0156297872271,-0.232742381310829,-0.0861971848975942));
#8132=CARTESIAN_POINT('Ctrl Pts',(1.01837060663223,-0.244234834628584,-0.0430711894098823));
#8133=CARTESIAN_POINT('Ctrl Pts',(1.019052,-0.246942143572133,-0.0206568624125607));
#8134=CARTESIAN_POINT('Ctrl Pts',(1.019052,-0.246942143572133,0.0206568624125607));
#8135=CARTESIAN_POINT('Ctrl Pts',(1.01837060663223,-0.244234834628584,0.0430711894098823));
#8136=CARTESIAN_POINT('Ctrl Pts',(1.0156297872271,-0.232742381310829,0.0861971848975942));
#8137=CARTESIAN_POINT('Ctrl Pts',(1.01358704779679,-0.223955109275652,0.106909345252087));
#8138=CARTESIAN_POINT('Ctrl Pts',(1.00869718865384,-0.201072148666545,0.1465689792446));
#8139=CARTESIAN_POINT('Ctrl Pts',(1.00492400591205,-0.181890537957859,0.169940289819232));
#8140=CARTESIAN_POINT('Ctrl Pts',(0.998375294985966,-0.141695629206859,
0.205111543747588));
#8141=CARTESIAN_POINT('Ctrl Pts',(0.994830026707808,-0.115492077056649,
0.221129100087819));
#8142=CARTESIAN_POINT('Ctrl Pts',(0.991238884025248,-0.0742967091364492,
0.236509675094874));
#8143=CARTESIAN_POINT('Ctrl Pts',(0.990332542620729,-0.0609922781173483,
0.24024064412003));
#8144=CARTESIAN_POINT('Ctrl Pts',(0.989696097314,-0.04763,0.242834539687907));
#8145=CARTESIAN_POINT('Origin',(0.,-0.04763,0.));
#8146=CARTESIAN_POINT('Origin',(0.,-0.04763,0.));
#8147=CARTESIAN_POINT('',(0.238183666596899,-0.04763,0.951592097314));
#8148=CARTESIAN_POINT('Origin',(0.,-0.04763,0.));
#8149=CARTESIAN_POINT('Origin',(-1.94289029309402E-16,-0.04763,1.));
#8150=CARTESIAN_POINT('Origin',(-1.94289029309402E-16,0.,1.));
#8151=CARTESIAN_POINT('',(-0.2381836665969,-0.04763,0.951592097314));
#8152=CARTESIAN_POINT('Ctrl Pts',(-0.238183666596899,-0.0476299999999999,
0.951592097314));
#8153=CARTESIAN_POINT('Ctrl Pts',(-0.233157223576062,-0.0740444353928835,
0.952850216871763));
#8154=CARTESIAN_POINT('Ctrl Pts',(-0.223801617934946,-0.0999305678883309,
0.955173119738174));
#8155=CARTESIAN_POINT('Ctrl Pts',(-0.199966927975188,-0.142345102874864,
0.960411259488514));
#8156=CARTESIAN_POINT('Ctrl Pts',(-0.1868781821531,-0.159766064500479,0.963103647174702));
#8157=CARTESIAN_POINT('Ctrl Pts',(-0.15681442133453,-0.190326085855194,
0.968453058988463));
#8158=CARTESIAN_POINT('Ctrl Pts',(-0.139836317888043,-0.203463743702801,
0.971100730005489));
#8159=CARTESIAN_POINT('Ctrl Pts',(-0.104422493053067,-0.224161999508995,
0.975530745318961));
#8160=CARTESIAN_POINT('Ctrl Pts',(-0.0842175114474176,-0.232861760990032,
0.977553872336861));
#8161=CARTESIAN_POINT('Ctrl Pts',(-0.0421062857595701,-0.244251601209411,
0.980270995488453));
#8162=CARTESIAN_POINT('Ctrl Pts',(-0.0201990724523197,-0.246942143572133,
0.980948));
#8163=CARTESIAN_POINT('Ctrl Pts',(0.020199072452319,-0.246942143572133,
0.980948));
#8164=CARTESIAN_POINT('Ctrl Pts',(0.0421062857595694,-0.244251601209411,
0.980270995488454));
#8165=CARTESIAN_POINT('Ctrl Pts',(0.0842175114474169,-0.232861760990032,
0.977553872336861));
#8166=CARTESIAN_POINT('Ctrl Pts',(0.104422493053067,-0.224161999508995,
0.975530745318961));
#8167=CARTESIAN_POINT('Ctrl Pts',(0.139836317888042,-0.203463743702801,
0.971100730005489));
#8168=CARTESIAN_POINT('Ctrl Pts',(0.15681442133453,-0.190326085855194,0.968453058988463));
#8169=CARTESIAN_POINT('Ctrl Pts',(0.1868781821531,-0.15976606450048,0.963103647174702));
#8170=CARTESIAN_POINT('Ctrl Pts',(0.199966927975188,-0.142345102874864,
0.960411259488514));
#8171=CARTESIAN_POINT('Ctrl Pts',(0.223801617934945,-0.0999305678883309,
0.955173119738174));
#8172=CARTESIAN_POINT('Ctrl Pts',(0.233157223576061,-0.0740444353928835,
0.952850216871763));
#8173=CARTESIAN_POINT('Ctrl Pts',(0.238183666596899,-0.0476299999999999,
0.951592097314));
#8174=CARTESIAN_POINT('Origin',(-1.94289029309402E-16,-0.04763,1.));
#8175=CARTESIAN_POINT('Origin',(0.,-0.04763,0.));
#8176=CARTESIAN_POINT('',(-0.504455939115715,-0.04763,0.841298510752802));
#8177=CARTESIAN_POINT('Origin',(0.,-0.04763,0.));
#8178=CARTESIAN_POINT('Origin',(-0.707106781186548,-0.04763,0.707106781186547));
#8179=CARTESIAN_POINT('Origin',(-0.707106781186548,0.,0.707106781186547));
#8180=CARTESIAN_POINT('',(-0.841298510752802,-0.04763,0.504455939115715));
#8181=CARTESIAN_POINT('Ctrl Pts',(-0.841298510752802,-0.04763,0.504455939115715));
#8182=CARTESIAN_POINT('Ctrl Pts',(-0.838633903678357,-0.0740444353928835,
0.508899795931835));
#8183=CARTESIAN_POINT('Ctrl Pts',(-0.833661031856294,-0.0999305678883309,
0.517157748491652));
#8184=CARTESIAN_POINT('Ctrl Pts',(-0.820511285096538,-0.142345102874864,
0.537715343527944));
#8185=CARTESIAN_POINT('Ctrl Pts',(-0.813159949759,-0.159766064500479,0.548874290046456));
#8186=CARTESIAN_POINT('Ctrl Pts',(-0.795684265985089,-0.190326085855194,
0.573915184558107));
#8187=CARTESIAN_POINT('Ctrl Pts',(-0.78555112003688,-0.203463743702801,
0.587792702767295));
#8188=CARTESIAN_POINT('Ctrl Pts',(-0.763642258217233,-0.224161999508995,
0.615966552324775));
#8189=CARTESIAN_POINT('Ctrl Pts',(-0.750785745543687,-0.232861760990032,
0.631684198665438));
#8190=CARTESIAN_POINT('Ctrl Pts',(-0.722929908501543,-0.244251601209411,
0.663382628119203));
#8191=CARTESIAN_POINT('Ctrl Pts',(-0.707917883896095,-0.246942143572133,
0.679352081686668));
#8192=CARTESIAN_POINT('Ctrl Pts',(-0.679352081686668,-0.246942143572133,
0.707917883896095));
#8193=CARTESIAN_POINT('Ctrl Pts',(-0.663382628119203,-0.244251601209411,
0.722929908501544));
#8194=CARTESIAN_POINT('Ctrl Pts',(-0.631684198665438,-0.232861760990031,
0.750785745543687));
#8195=CARTESIAN_POINT('Ctrl Pts',(-0.615966552324775,-0.224161999508995,
0.763642258217233));
#8196=CARTESIAN_POINT('Ctrl Pts',(-0.587792702767295,-0.203463743702801,
0.78555112003688));
#8197=CARTESIAN_POINT('Ctrl Pts',(-0.573915184558107,-0.190326085855194,
0.795684265985088));
#8198=CARTESIAN_POINT('Ctrl Pts',(-0.548874290046456,-0.159766064500479,
0.813159949759));
#8199=CARTESIAN_POINT('Ctrl Pts',(-0.537715343527944,-0.142345102874864,
0.820511285096538));
#8200=CARTESIAN_POINT('Ctrl Pts',(-0.517157748491652,-0.0999305678883309,
0.833661031856294));
#8201=CARTESIAN_POINT('Ctrl Pts',(-0.508899795931835,-0.0740444353928835,
0.838633903678357));
#8202=CARTESIAN_POINT('Ctrl Pts',(-0.504455939115716,-0.04763,0.841298510752801));
#8203=CARTESIAN_POINT('Origin',(-0.707106781186548,-0.04763,0.707106781186547));
#8204=CARTESIAN_POINT('Origin',(0.,-0.04763,0.));
#8205=CARTESIAN_POINT('',(-0.951592097314,-0.04763,0.238183666596899));
#8206=CARTESIAN_POINT('Origin',(0.,-0.04763,0.));
#8207=CARTESIAN_POINT('Origin',(-1.,-0.04763,-1.11022302462516E-16));
#8208=CARTESIAN_POINT('Origin',(-1.,0.,-1.11022302462516E-16));
#8209=CARTESIAN_POINT('',(-0.951592097314,-0.04763,-0.2381836665969));
#8210=CARTESIAN_POINT('',(-0.980948,-0.246942143572133,1.08514323328844E-18));
#8211=CARTESIAN_POINT('Ctrl Pts',(-0.951592097314,-0.04763,-0.238183666596899));
#8212=CARTESIAN_POINT('Ctrl Pts',(-0.952850216871763,-0.0740444353928835,
-0.233157223576062));
#8213=CARTESIAN_POINT('Ctrl Pts',(-0.955173119738174,-0.0999305678883309,
-0.223801617934946));
#8214=CARTESIAN_POINT('Ctrl Pts',(-0.960411259488514,-0.142345102874864,
-0.199966927975188));
#8215=CARTESIAN_POINT('Ctrl Pts',(-0.963103647174702,-0.159766064500479,
-0.1868781821531));
#8216=CARTESIAN_POINT('Ctrl Pts',(-0.968453058988463,-0.190326085855194,
-0.15681442133453));
#8217=CARTESIAN_POINT('Ctrl Pts',(-0.971100730005489,-0.203463743702801,
-0.139836317888043));
#8218=CARTESIAN_POINT('Ctrl Pts',(-0.975530745318961,-0.224161999508995,
-0.104422493053067));
#8219=CARTESIAN_POINT('Ctrl Pts',(-0.977553872336861,-0.232861760990032,
-0.0842175114474175));
#8220=CARTESIAN_POINT('Ctrl Pts',(-0.980270995488453,-0.244251601209411,
-0.0421062857595699));
#8221=CARTESIAN_POINT('Ctrl Pts',(-0.980948,-0.246942143572133,-0.0201990724523195));
#8222=CARTESIAN_POINT('Ctrl Pts',(-0.980948,-0.246942143572133,-1.17961196366423E-16));
#8223=CARTESIAN_POINT('Origin',(-1.,-0.04763,-1.11022302462516E-16));
#8224=CARTESIAN_POINT('Ctrl Pts',(-0.980948,-0.246942143572133,-1.17961196366423E-16));
#8225=CARTESIAN_POINT('Ctrl Pts',(-0.980948,-0.246942143572133,0.0201990724523192));
#8226=CARTESIAN_POINT('Ctrl Pts',(-0.980270995488453,-0.244251601209411,
0.0421062857595695));
#8227=CARTESIAN_POINT('Ctrl Pts',(-0.977553872336861,-0.232861760990032,
0.0842175114474169));
#8228=CARTESIAN_POINT('Ctrl Pts',(-0.975530745318961,-0.224161999508995,
0.104422493053066));
#8229=CARTESIAN_POINT('Ctrl Pts',(-0.971100730005489,-0.203463743702801,
0.139836317888042));
#8230=CARTESIAN_POINT('Ctrl Pts',(-0.968453058988463,-0.190326085855194,
0.15681442133453));
#8231=CARTESIAN_POINT('Ctrl Pts',(-0.963103647174702,-0.15976606450048,
0.1868781821531));
#8232=CARTESIAN_POINT('Ctrl Pts',(-0.960411259488514,-0.142345102874864,
0.199966927975188));
#8233=CARTESIAN_POINT('Ctrl Pts',(-0.955173119738174,-0.099930567888331,
0.223801617934945));
#8234=CARTESIAN_POINT('Ctrl Pts',(-0.952850216871763,-0.0740444353928835,
0.233157223576061));
#8235=CARTESIAN_POINT('Ctrl Pts',(-0.951592097314,-0.04763,0.238183666596899));
#8236=CARTESIAN_POINT('Origin',(0.,-0.04763,0.));
#8237=CARTESIAN_POINT('',(-0.841298510752802,-0.04763,-0.504455939115715));
#8238=CARTESIAN_POINT('Origin',(0.,-0.04763,0.));
#8239=CARTESIAN_POINT('Origin',(-0.707106781186547,-0.04763,-0.707106781186548));
#8240=CARTESIAN_POINT('Origin',(-0.707106781186547,0.,-0.707106781186548));
#8241=CARTESIAN_POINT('',(-0.504455939115715,-0.04763,-0.841298510752802));
#8242=CARTESIAN_POINT('Ctrl Pts',(-0.504455939115715,-0.04763,-0.841298510752802));
#8243=CARTESIAN_POINT('Ctrl Pts',(-0.508899795931835,-0.0740444353928835,
-0.838633903678357));
#8244=CARTESIAN_POINT('Ctrl Pts',(-0.517157748491652,-0.0999305678883309,
-0.833661031856294));
#8245=CARTESIAN_POINT('Ctrl Pts',(-0.537715343527944,-0.142345102874864,
-0.820511285096538));
#8246=CARTESIAN_POINT('Ctrl Pts',(-0.548874290046456,-0.159766064500479,
-0.813159949759));
#8247=CARTESIAN_POINT('Ctrl Pts',(-0.573915184558107,-0.190326085855194,
-0.795684265985089));
#8248=CARTESIAN_POINT('Ctrl Pts',(-0.587792702767295,-0.203463743702801,
-0.78555112003688));
#8249=CARTESIAN_POINT('Ctrl Pts',(-0.615966552324775,-0.224161999508995,
-0.763642258217233));
#8250=CARTESIAN_POINT('Ctrl Pts',(-0.631684198665438,-0.232861760990032,
-0.750785745543687));
#8251=CARTESIAN_POINT('Ctrl Pts',(-0.663382628119203,-0.244251601209411,
-0.722929908501543));
#8252=CARTESIAN_POINT('Ctrl Pts',(-0.679352081686668,-0.246942143572133,
-0.707917883896095));
#8253=CARTESIAN_POINT('Ctrl Pts',(-0.707917883896095,-0.246942143572133,
-0.679352081686668));
#8254=CARTESIAN_POINT('Ctrl Pts',(-0.722929908501543,-0.244251601209411,
-0.663382628119203));
#8255=CARTESIAN_POINT('Ctrl Pts',(-0.750785745543687,-0.232861760990032,
-0.631684198665439));
#8256=CARTESIAN_POINT('Ctrl Pts',(-0.763642258217232,-0.224161999508995,
-0.615966552324775));
#8257=CARTESIAN_POINT('Ctrl Pts',(-0.78555112003688,-0.203463743702801,
-0.587792702767295));
#8258=CARTESIAN_POINT('Ctrl Pts',(-0.795684265985088,-0.190326085855194,
-0.573915184558107));
#8259=CARTESIAN_POINT('Ctrl Pts',(-0.813159949759,-0.15976606450048,-0.548874290046456));
#8260=CARTESIAN_POINT('Ctrl Pts',(-0.820511285096538,-0.142345102874864,
-0.537715343527944));
#8261=CARTESIAN_POINT('Ctrl Pts',(-0.833661031856294,-0.0999305678883311,
-0.517157748491652));
#8262=CARTESIAN_POINT('Ctrl Pts',(-0.838633903678357,-0.0740444353928836,
-0.508899795931835));
#8263=CARTESIAN_POINT('Ctrl Pts',(-0.841298510752801,-0.04763,-0.504455939115715));
#8264=CARTESIAN_POINT('Origin',(-0.707106781186547,-0.04763,-0.707106781186548));
#8265=CARTESIAN_POINT('Origin',(0.,-0.04763,0.));
#8266=CARTESIAN_POINT('',(-0.238183666596899,-0.04763,-0.951592097314));
#8267=CARTESIAN_POINT('Origin',(0.,-0.04763,0.));
#8268=CARTESIAN_POINT('Origin',(5.55111512312578E-17,-0.04763,-1.));
#8269=CARTESIAN_POINT('Origin',(5.55111512312578E-17,0.,-1.));
#8270=CARTESIAN_POINT('',(0.238183666596899,-0.04763,-0.951592097314));
#8271=CARTESIAN_POINT('Ctrl Pts',(0.238183666596899,-0.04763,-0.951592097314));
#8272=CARTESIAN_POINT('Ctrl Pts',(0.233157223576062,-0.0740444353928835,
-0.952850216871763));
#8273=CARTESIAN_POINT('Ctrl Pts',(0.223801617934946,-0.099930567888331,
-0.955173119738174));
#8274=CARTESIAN_POINT('Ctrl Pts',(0.199966927975188,-0.142345102874864,
-0.960411259488514));
#8275=CARTESIAN_POINT('Ctrl Pts',(0.1868781821531,-0.15976606450048,-0.963103647174702));
#8276=CARTESIAN_POINT('Ctrl Pts',(0.15681442133453,-0.190326085855194,-0.968453058988463));
#8277=CARTESIAN_POINT('Ctrl Pts',(0.139836317888042,-0.203463743702801,
-0.971100730005489));
#8278=CARTESIAN_POINT('Ctrl Pts',(0.104422493053067,-0.224161999508995,
-0.975530745318961));
#8279=CARTESIAN_POINT('Ctrl Pts',(0.0842175114474173,-0.232861760990032,
-0.977553872336861));
#8280=CARTESIAN_POINT('Ctrl Pts',(0.0421062857595698,-0.244251601209411,
-0.980270995488453));
#8281=CARTESIAN_POINT('Ctrl Pts',(0.0201990724523194,-0.246942143572133,
-0.980948));
#8282=CARTESIAN_POINT('Ctrl Pts',(-0.0201990724523193,-0.246942143572133,
-0.980948));
#8283=CARTESIAN_POINT('Ctrl Pts',(-0.0421062857595697,-0.244251601209411,
-0.980270995488453));
#8284=CARTESIAN_POINT('Ctrl Pts',(-0.0842175114474171,-0.232861760990032,
-0.977553872336861));
#8285=CARTESIAN_POINT('Ctrl Pts',(-0.104422493053067,-0.224161999508995,
-0.975530745318961));
#8286=CARTESIAN_POINT('Ctrl Pts',(-0.139836317888042,-0.203463743702801,
-0.971100730005489));
#8287=CARTESIAN_POINT('Ctrl Pts',(-0.15681442133453,-0.190326085855194,
-0.968453058988463));
#8288=CARTESIAN_POINT('Ctrl Pts',(-0.1868781821531,-0.15976606450048,-0.963103647174702));
#8289=CARTESIAN_POINT('Ctrl Pts',(-0.199966927975188,-0.142345102874864,
-0.960411259488514));
#8290=CARTESIAN_POINT('Ctrl Pts',(-0.223801617934945,-0.099930567888331,
-0.955173119738174));
#8291=CARTESIAN_POINT('Ctrl Pts',(-0.233157223576062,-0.0740444353928835,
-0.952850216871763));
#8292=CARTESIAN_POINT('Ctrl Pts',(-0.238183666596899,-0.0476299999999999,
-0.951592097314));
#8293=CARTESIAN_POINT('Origin',(5.55111512312578E-17,-0.04763,-1.));
#8294=CARTESIAN_POINT('Origin',(0.,-0.04763,0.));
#8295=CARTESIAN_POINT('',(0.504455939115715,-0.04763,-0.841298510752802));
#8296=CARTESIAN_POINT('Origin',(0.,-0.04763,0.));
#8297=CARTESIAN_POINT('Origin',(0.707106781186548,-0.04763,-0.707106781186547));
#8298=CARTESIAN_POINT('Origin',(0.707106781186548,0.,-0.707106781186547));
#8299=CARTESIAN_POINT('',(0.841298510752802,-0.04763,-0.504455939115715));
#8300=CARTESIAN_POINT('Ctrl Pts',(0.841298510752802,-0.04763,-0.504455939115715));
#8301=CARTESIAN_POINT('Ctrl Pts',(0.838633903678357,-0.0740444353928835,
-0.508899795931835));
#8302=CARTESIAN_POINT('Ctrl Pts',(0.833661031856294,-0.0999305678883309,
-0.517157748491652));
#8303=CARTESIAN_POINT('Ctrl Pts',(0.820511285096538,-0.142345102874864,
-0.537715343527944));
#8304=CARTESIAN_POINT('Ctrl Pts',(0.813159949759,-0.159766064500479,-0.548874290046456));
#8305=CARTESIAN_POINT('Ctrl Pts',(0.795684265985088,-0.190326085855194,
-0.573915184558107));
#8306=CARTESIAN_POINT('Ctrl Pts',(0.78555112003688,-0.203463743702801,-0.587792702767295));
#8307=CARTESIAN_POINT('Ctrl Pts',(0.763642258217233,-0.224161999508995,
-0.615966552324775));
#8308=CARTESIAN_POINT('Ctrl Pts',(0.750785745543687,-0.232861760990032,
-0.631684198665438));
#8309=CARTESIAN_POINT('Ctrl Pts',(0.722929908501543,-0.244251601209411,
-0.663382628119203));
#8310=CARTESIAN_POINT('Ctrl Pts',(0.707917883896095,-0.246942143572133,
-0.679352081686668));
#8311=CARTESIAN_POINT('Ctrl Pts',(0.679352081686668,-0.246942143572133,
-0.707917883896095));
#8312=CARTESIAN_POINT('Ctrl Pts',(0.663382628119203,-0.244251601209411,
-0.722929908501543));
#8313=CARTESIAN_POINT('Ctrl Pts',(0.631684198665438,-0.232861760990032,
-0.750785745543687));
#8314=CARTESIAN_POINT('Ctrl Pts',(0.615966552324775,-0.224161999508995,
-0.763642258217232));
#8315=CARTESIAN_POINT('Ctrl Pts',(0.587792702767295,-0.203463743702801,
-0.78555112003688));
#8316=CARTESIAN_POINT('Ctrl Pts',(0.573915184558107,-0.190326085855194,
-0.795684265985088));
#8317=CARTESIAN_POINT('Ctrl Pts',(0.548874290046456,-0.159766064500479,
-0.813159949759));
#8318=CARTESIAN_POINT('Ctrl Pts',(0.537715343527944,-0.142345102874864,
-0.820511285096538));
#8319=CARTESIAN_POINT('Ctrl Pts',(0.517157748491652,-0.099930567888331,
-0.833661031856294));
#8320=CARTESIAN_POINT('Ctrl Pts',(0.508899795931835,-0.0740444353928835,
-0.838633903678357));
#8321=CARTESIAN_POINT('Ctrl Pts',(0.504455939115715,-0.04763,-0.841298510752801));
#8322=CARTESIAN_POINT('Origin',(0.707106781186548,-0.04763,-0.707106781186547));
#8323=CARTESIAN_POINT('Origin',(0.,-0.166705,0.));
#8324=CARTESIAN_POINT('',(-0.980948,-0.28578,1.20131482833E-16));
#8325=CARTESIAN_POINT('Origin',(0.,-0.28578,0.));
#8326=CARTESIAN_POINT('',(-0.980948,-0.166705,1.20131482833E-16));
#8327=CARTESIAN_POINT('',(0.951592097314,-0.04763,0.238183666596899));
#8328=CARTESIAN_POINT('Origin',(0.,-0.04763,0.));
#8329=CARTESIAN_POINT('',(0.951592097314,-0.04763,-0.238183666596899));
#8330=CARTESIAN_POINT('Ctrl Pts',(0.951592097314,-0.04763,0.238183666596899));
#8331=CARTESIAN_POINT('Ctrl Pts',(0.952850216871763,-0.0740444353928835,
0.233157223576062));
#8332=CARTESIAN_POINT('Ctrl Pts',(0.955173119738174,-0.099930567888331,
0.223801617934945));
#8333=CARTESIAN_POINT('Ctrl Pts',(0.960411259488514,-0.142345102874864,
0.199966927975188));
#8334=CARTESIAN_POINT('Ctrl Pts',(0.963103647174702,-0.15976606450048,0.1868781821531));
#8335=CARTESIAN_POINT('Ctrl Pts',(0.968453058988463,-0.190326085855194,
0.15681442133453));
#8336=CARTESIAN_POINT('Ctrl Pts',(0.971100730005489,-0.203463743702801,
0.139836317888042));
#8337=CARTESIAN_POINT('Ctrl Pts',(0.975530745318961,-0.224161999508995,
0.104422493053067));
#8338=CARTESIAN_POINT('Ctrl Pts',(0.977553872336861,-0.232861760990032,
0.0842175114474172));
#8339=CARTESIAN_POINT('Ctrl Pts',(0.980270995488453,-0.244251601209411,
0.0421062857595697));
#8340=CARTESIAN_POINT('Ctrl Pts',(0.980948,-0.246942143572133,0.0201990724523194));
#8341=CARTESIAN_POINT('Ctrl Pts',(0.980948,-0.246942143572133,-0.0201990724523194));
#8342=CARTESIAN_POINT('Ctrl Pts',(0.980270995488453,-0.244251601209411,
-0.0421062857595697));
#8343=CARTESIAN_POINT('Ctrl Pts',(0.977553872336861,-0.232861760990032,
-0.0842175114474172));
#8344=CARTESIAN_POINT('Ctrl Pts',(0.975530745318961,-0.224161999508995,
-0.104422493053067));
#8345=CARTESIAN_POINT('Ctrl Pts',(0.971100730005489,-0.203463743702801,
-0.139836317888042));
#8346=CARTESIAN_POINT('Ctrl Pts',(0.968453058988463,-0.190326085855194,
-0.15681442133453));
#8347=CARTESIAN_POINT('Ctrl Pts',(0.963103647174702,-0.15976606450048,-0.1868781821531));
#8348=CARTESIAN_POINT('Ctrl Pts',(0.960411259488514,-0.142345102874864,
-0.199966927975188));
#8349=CARTESIAN_POINT('Ctrl Pts',(0.955173119738174,-0.099930567888331,
-0.223801617934945));
#8350=CARTESIAN_POINT('Ctrl Pts',(0.952850216871763,-0.0740444353928835,
-0.233157223576062));
#8351=CARTESIAN_POINT('Ctrl Pts',(0.951592097314,-0.0476299999999999,-0.238183666596899));
#8352=CARTESIAN_POINT('Origin',(0.,-0.04763,0.));
#8353=CARTESIAN_POINT('Origin',(0.,-0.04763,0.));
#8354=CARTESIAN_POINT('Origin',(1.,-0.04763,0.));
#8355=CARTESIAN_POINT('Origin',(1.,0.,0.));
#8356=CARTESIAN_POINT('Origin',(1.,-0.04763,0.));
#8357=CARTESIAN_POINT('Origin',(0.,-0.28578,0.));
#8358=CARTESIAN_POINT('Origin',(0.,-0.04763,0.));
#8359=CARTESIAN_POINT('',(0.,0.,0.));
#8360=CARTESIAN_POINT('Origin',(1.013815,0.445,0.));
#8361=CARTESIAN_POINT('',(-1.013815,0.445,-1.24156529467757E-16));
#8362=CARTESIAN_POINT('Origin',(0.,0.445,0.));
#8363=CARTESIAN_POINT('',(-0.991185,0.445,-1.21385153761287E-16));
#8364=CARTESIAN_POINT('Origin',(0.,0.445,0.));
#8365=CARTESIAN_POINT('Origin',(0.,0.4075,0.));
#8366=CARTESIAN_POINT('',(-1.013815,0.37,-1.24156529467757E-16));
#8367=CARTESIAN_POINT('Origin',(0.,0.37,0.));
#8368=CARTESIAN_POINT('',(-1.013815,0.4075,-1.24156529467757E-16));
#8369=CARTESIAN_POINT('Origin',(0.991185,0.37,0.));
#8370=CARTESIAN_POINT('',(-0.991185,0.37,-1.21385153761287E-16));
#8371=CARTESIAN_POINT('Origin',(0.,0.37,0.));
#8372=CARTESIAN_POINT('Origin',(0.,0.4075,0.));
#8373=CARTESIAN_POINT('',(-0.991185,0.4075,-1.21385153761287E-16));
#8374=CARTESIAN_POINT('Origin',(1.013815,-0.37,0.));
#8375=CARTESIAN_POINT('',(-1.013815,-0.37,-1.24156529467757E-16));
#8376=CARTESIAN_POINT('Origin',(0.,-0.37,0.));
#8377=CARTESIAN_POINT('',(-0.991185,-0.37,-1.21385153761287E-16));
#8378=CARTESIAN_POINT('Origin',(0.,-0.37,0.));
#8379=CARTESIAN_POINT('Origin',(0.,-0.4075,0.));
#8380=CARTESIAN_POINT('',(-1.013815,-0.445,-1.24156529467757E-16));
#8381=CARTESIAN_POINT('Origin',(0.,-0.445,0.));
#8382=CARTESIAN_POINT('',(-1.013815,-0.4075,-1.24156529467757E-16));
#8383=CARTESIAN_POINT('Origin',(0.991185,-0.445,0.));
#8384=CARTESIAN_POINT('',(-0.991185,-0.445,-1.21385153761287E-16));
#8385=CARTESIAN_POINT('Origin',(0.,-0.445,0.));
#8386=CARTESIAN_POINT('Origin',(0.,-0.4075,0.));
#8387=CARTESIAN_POINT('',(-0.991185,-0.4075,-1.21385153761287E-16));
#8388=CARTESIAN_POINT('',(0.,0.,0.));
#8389=CARTESIAN_POINT('',(0.,0.,0.));
#8390=CARTESIAN_POINT('',(0.,0.,0.));
#8391=CARTESIAN_POINT('',(0.,0.,0.));
#8392=CARTESIAN_POINT('',(0.,0.,0.));
#8393=CARTESIAN_POINT('',(0.,0.,0.));
#8394=CARTESIAN_POINT('Origin',(1.5,-2.,2.8));
#8395=CARTESIAN_POINT('',(1.84003676271839,-2.4,6.5));
#8396=CARTESIAN_POINT('',(1.84003676271839,-2.4,2.8));
#8397=CARTESIAN_POINT('',(1.84003676271839,-2.4,2.8));
#8398=CARTESIAN_POINT('',(1.84003676271839,-1.6,6.5));
#8399=CARTESIAN_POINT('Origin',(1.5,-2.,6.5));
#8400=CARTESIAN_POINT('',(1.84003676271839,-1.6,2.8));
#8401=CARTESIAN_POINT('',(1.84003676271839,-1.6,2.8));
#8402=CARTESIAN_POINT('Origin',(1.5,-2.,2.8));
#8403=CARTESIAN_POINT('Origin',(1.5,-2.,2.8));
#8404=CARTESIAN_POINT('',(1.15996323728161,-2.4,2.8));
#8405=CARTESIAN_POINT('',(1.15996323728161,-2.4,6.5));
#8406=CARTESIAN_POINT('',(1.15996323728161,-2.4,2.8));
#8407=CARTESIAN_POINT('',(1.15996323728161,-1.6,2.8));
#8408=CARTESIAN_POINT('Origin',(1.5,-2.,2.8));
#8409=CARTESIAN_POINT('',(1.15996323728161,-1.6,6.5));
#8410=CARTESIAN_POINT('',(1.15996323728161,-1.6,2.8));
#8411=CARTESIAN_POINT('Origin',(1.5,-2.,6.5));
#8412=CARTESIAN_POINT('Origin',(0.,-2.4,4.6));
#8413=CARTESIAN_POINT('',(2.2,-2.4,2.8));
#8414=CARTESIAN_POINT('',(0.,-2.4,2.8));
#8415=CARTESIAN_POINT('',(2.2,-2.4,6.5));
#8416=CARTESIAN_POINT('',(2.2,-2.4,2.7));
#8417=CARTESIAN_POINT('',(2.2,-2.4,6.5));
#8418=CARTESIAN_POINT('Origin',(0.,-2.4,4.6));
#8419=CARTESIAN_POINT('',(-1.15996323728161,-2.4,6.5));
#8420=CARTESIAN_POINT('',(2.2,-2.4,6.5));
#8421=CARTESIAN_POINT('',(-1.15996323728161,-2.4,2.8));
#8422=CARTESIAN_POINT('',(-1.15996323728161,-2.4,2.8));
#8423=CARTESIAN_POINT('',(0.,-2.4,2.8));
#8424=CARTESIAN_POINT('',(-0.505,-2.4,4.5));
#8425=CARTESIAN_POINT('Origin',(0.,-2.4,4.5));
#8426=CARTESIAN_POINT('Origin',(-2.2,-2.4,6.5));
#8427=CARTESIAN_POINT('',(2.2,-1.6,6.5));
#8428=CARTESIAN_POINT('',(2.2,-2.4,6.5));
#8429=CARTESIAN_POINT('',(2.2,-1.6,6.5));
#8430=CARTESIAN_POINT('Origin',(-2.2,-2.4,6.5));
#8431=CARTESIAN_POINT('',(-1.15996323728161,-1.6,6.5));
#8432=CARTESIAN_POINT('',(2.2,-1.6,6.5));
#8433=CARTESIAN_POINT('Origin',(-1.5,-2.,6.5));
#8434=CARTESIAN_POINT('Origin',(0.,-1.6,4.6));
#8435=CARTESIAN_POINT('',(2.2,-1.6,2.8));
#8436=CARTESIAN_POINT('',(2.2,-1.6,2.7));
#8437=CARTESIAN_POINT('',(0.,-1.6,2.8));
#8438=CARTESIAN_POINT('Origin',(0.,-1.6,4.6));
#8439=CARTESIAN_POINT('',(-1.15996323728161,-1.6,2.8));
#8440=CARTESIAN_POINT('',(0.,-1.6,2.8));
#8441=CARTESIAN_POINT('',(-1.15996323728161,-1.6,2.8));
#8442=CARTESIAN_POINT('',(-0.505,-1.6,4.5));
#8443=CARTESIAN_POINT('Origin',(0.,-1.6,4.5));
#8444=CARTESIAN_POINT('Origin',(1.5,-2.,1.9));
#8445=CARTESIAN_POINT('',(1.225,-2.,2.));
#8446=CARTESIAN_POINT('Origin',(1.5,-2.,2.));
#8447=CARTESIAN_POINT('',(1.225,-2.,2.8));
#8448=CARTESIAN_POINT('',(1.225,-2.,1.9));
#8449=CARTESIAN_POINT('Origin',(1.5,-2.,2.8));
#8450=CARTESIAN_POINT('Origin',(-1.5,-2.,2.8));
#8451=CARTESIAN_POINT('',(-1.84003676271839,-1.6,6.5));
#8452=CARTESIAN_POINT('',(-1.84003676271839,-1.6,2.8));
#8453=CARTESIAN_POINT('',(-1.84003676271839,-1.6,2.8));
#8454=CARTESIAN_POINT('',(-1.84003676271839,-2.4,6.5));
#8455=CARTESIAN_POINT('Origin',(-1.5,-2.,6.5));
#8456=CARTESIAN_POINT('',(-1.84003676271839,-2.4,2.8));
#8457=CARTESIAN_POINT('',(-1.84003676271839,-2.4,2.8));
#8458=CARTESIAN_POINT('Origin',(-1.5,-2.,2.8));
#8459=CARTESIAN_POINT('Origin',(-1.5,-2.,2.8));
#8460=CARTESIAN_POINT('Origin',(-1.5,-2.,2.8));
#8461=CARTESIAN_POINT('Origin',(0.,-1.6,4.6));
#8462=CARTESIAN_POINT('',(-2.2,-1.6,2.8));
#8463=CARTESIAN_POINT('',(0.,-1.6,2.8));
#8464=CARTESIAN_POINT('',(-2.2,-1.6,6.5));
#8465=CARTESIAN_POINT('',(-2.2,-1.6,6.5));
#8466=CARTESIAN_POINT('',(2.2,-1.6,6.5));
#8467=CARTESIAN_POINT('Origin',(-2.2,-2.4,6.5));
#8468=CARTESIAN_POINT('',(-2.2,-2.4,6.5));
#8469=CARTESIAN_POINT('',(-2.2,-2.4,6.5));
#8470=CARTESIAN_POINT('',(2.2,-2.4,6.5));
#8471=CARTESIAN_POINT('Origin',(0.,-2.4,4.6));
#8472=CARTESIAN_POINT('',(-2.2,-2.4,2.8));
#8473=CARTESIAN_POINT('',(-2.2,-2.4,6.5));
#8474=CARTESIAN_POINT('',(0.,-2.4,2.8));
#8475=CARTESIAN_POINT('Origin',(-1.5,-2.,1.9));
#8476=CARTESIAN_POINT('',(-1.775,-2.,2.));
#8477=CARTESIAN_POINT('Origin',(-1.5,-2.,2.));
#8478=CARTESIAN_POINT('',(-1.775,-2.,2.8));
#8479=CARTESIAN_POINT('',(-1.775,-2.,1.9));
#8480=CARTESIAN_POINT('Origin',(-1.5,-2.,2.8));
#8481=CARTESIAN_POINT('Origin',(0.,-2.5,4.5));
#8482=CARTESIAN_POINT('',(-0.505,-2.5,4.5));
#8483=CARTESIAN_POINT('Origin',(2.2,-2.4,6.5));
#8484=CARTESIAN_POINT('',(2.2,-2.2,2.8));
#8485=CARTESIAN_POINT('Origin',(-2.2,-2.4,2.7));
#8486=CARTESIAN_POINT('',(-2.2,-2.2,2.8));
#8487=CARTESIAN_POINT('Origin',(3.,-0.8,2.));
#8488=CARTESIAN_POINT('',(3.,-0.8,2.));
#8489=CARTESIAN_POINT('',(-3.,-0.8,2.));
#8490=CARTESIAN_POINT('',(3.,-0.8,2.));
#8491=CARTESIAN_POINT('',(-3.,-0.8,2.8));
#8492=CARTESIAN_POINT('',(-3.,-0.8,2.));
#8493=CARTESIAN_POINT('',(3.,-0.8,2.8));
#8494=CARTESIAN_POINT('',(3.,-0.8,2.8));
#8495=CARTESIAN_POINT('',(3.,-0.8,2.));
#8496=CARTESIAN_POINT('Origin',(3.,-3.2,2.));
#8497=CARTESIAN_POINT('',(3.,-3.2,2.));
#8498=CARTESIAN_POINT('',(3.,-3.2,2.));
#8499=CARTESIAN_POINT('',(3.,-3.2,2.8));
#8500=CARTESIAN_POINT('',(3.,-3.2,2.8));
#8501=CARTESIAN_POINT('',(3.,-3.2,2.));
#8502=CARTESIAN_POINT('Origin',(-3.,-3.2,2.));
#8503=CARTESIAN_POINT('',(-3.,-3.2,2.));
#8504=CARTESIAN_POINT('',(-3.,-3.2,2.));
#8505=CARTESIAN_POINT('',(-3.,-3.2,2.8));
#8506=CARTESIAN_POINT('',(-3.,-3.2,2.8));
#8507=CARTESIAN_POINT('',(-3.,-3.2,2.));
#8508=CARTESIAN_POINT('Origin',(-3.,-0.8,2.));
#8509=CARTESIAN_POINT('',(-3.,-0.8,2.));
#8510=CARTESIAN_POINT('',(-3.,-0.8,2.8));
#8511=CARTESIAN_POINT('Origin',(0.,-2.,2.8));
#8512=CARTESIAN_POINT('Origin',(0.,-2.,2.));
#8513=CARTESIAN_POINT('',(0.,0.,0.));
#8514=CARTESIAN_POINT('Origin',(-3.5,-2.,1.9));
#8515=CARTESIAN_POINT('',(-3.775,-2.,2.));
#8516=CARTESIAN_POINT('Origin',(-3.5,-2.,2.));
#8517=CARTESIAN_POINT('',(-3.775,-2.,2.8));
#8518=CARTESIAN_POINT('',(-3.775,-2.,1.9));
#8519=CARTESIAN_POINT('Origin',(-3.5,-2.,2.8));
#8520=CARTESIAN_POINT('Origin',(-5.1,-2.,4.5));
#8521=CARTESIAN_POINT('',(-5.,-2.,4.84));
#8522=CARTESIAN_POINT('Origin',(-5.,-2.,4.5));
#8523=CARTESIAN_POINT('',(-4.2,-2.,4.84));
#8524=CARTESIAN_POINT('',(-5.1,-2.,4.84));
#8525=CARTESIAN_POINT('Origin',(-4.2,-2.,4.5));
#8526=CARTESIAN_POINT('Origin',(-5.,-0.8,5.5));
#8527=CARTESIAN_POINT('',(-5.,-0.8,5.5));
#8528=CARTESIAN_POINT('',(-5.,-3.2,5.5));
#8529=CARTESIAN_POINT('',(-5.,-0.8,5.5));
#8530=CARTESIAN_POINT('',(-4.2,-3.2,5.5));
#8531=CARTESIAN_POINT('',(-5.,-3.2,5.5));
#8532=CARTESIAN_POINT('',(-4.2,-0.8,5.5));
#8533=CARTESIAN_POINT('',(-4.2,-0.8,5.5));
#8534=CARTESIAN_POINT('',(-5.,-0.8,5.5));
#8535=CARTESIAN_POINT('Origin',(-4.2,-2.,4.1));
#8536=CARTESIAN_POINT('',(-4.2,-0.8,2.8));
#8537=CARTESIAN_POINT('',(-4.2,-3.2,2.8));
#8538=CARTESIAN_POINT('',(-4.2,-2.,2.8));
#8539=CARTESIAN_POINT('',(-4.2,-0.8,2.7));
#8540=CARTESIAN_POINT('',(-4.2,-3.2,5.5));
#8541=CARTESIAN_POINT('Origin',(-4.,-2.,2.8));
#8542=CARTESIAN_POINT('',(-3.,-3.2,2.8));
#8543=CARTESIAN_POINT('',(-5.,-3.2,2.8));
#8544=CARTESIAN_POINT('',(-3.,-0.8,2.8));
#8545=CARTESIAN_POINT('',(-3.,-3.2,2.8));
#8546=CARTESIAN_POINT('',(-3.,-0.8,2.8));
#8547=CARTESIAN_POINT('Origin',(-5.,-3.2,2.));
#8548=CARTESIAN_POINT('',(-5.,-3.2,2.));
#8549=CARTESIAN_POINT('',(-5.,-3.2,2.));
#8550=CARTESIAN_POINT('',(-3.,-3.2,2.));
#8551=CARTESIAN_POINT('',(-5.,-3.2,2.));
#8552=CARTESIAN_POINT('',(-3.,-3.2,2.));
#8553=CARTESIAN_POINT('Origin',(-3.,-0.8,2.));
#8554=CARTESIAN_POINT('',(-3.,-0.8,2.));
#8555=CARTESIAN_POINT('',(-3.,-0.8,2.));
#8556=CARTESIAN_POINT('',(-5.,-0.8,2.));
#8557=CARTESIAN_POINT('',(-3.,-0.8,2.));
#8558=CARTESIAN_POINT('',(-5.,-0.8,2.));
#8559=CARTESIAN_POINT('Origin',(-3.,-3.2,2.));
#8560=CARTESIAN_POINT('',(-3.,-3.2,2.));
#8561=CARTESIAN_POINT('Origin',(-5.,-0.8,2.));
#8562=CARTESIAN_POINT('',(-5.,-0.8,2.));
#8563=CARTESIAN_POINT('Origin',(-4.,-2.,2.));
#8564=CARTESIAN_POINT('',(0.,0.,0.));
#8565=CARTESIAN_POINT('Origin',(1.5,32.,2.8));
#8566=CARTESIAN_POINT('',(1.84003676271839,31.6,6.5));
#8567=CARTESIAN_POINT('',(1.84003676271839,31.6,2.8));
#8568=CARTESIAN_POINT('',(1.84003676271839,31.6,2.8));
#8569=CARTESIAN_POINT('',(1.84003676271839,32.4,6.5));
#8570=CARTESIAN_POINT('Origin',(1.5,32.,6.5));
#8571=CARTESIAN_POINT('',(1.84003676271839,32.4,2.8));
#8572=CARTESIAN_POINT('',(1.84003676271839,32.4,2.8));
#8573=CARTESIAN_POINT('Origin',(1.5,32.,2.8));
#8574=CARTESIAN_POINT('Origin',(1.5,32.,2.8));
#8575=CARTESIAN_POINT('',(1.15996323728161,31.6,2.8));
#8576=CARTESIAN_POINT('',(1.15996323728161,31.6,6.5));
#8577=CARTESIAN_POINT('',(1.15996323728161,31.6,2.8));
#8578=CARTESIAN_POINT('',(1.15996323728161,32.4,2.8));
#8579=CARTESIAN_POINT('Origin',(1.5,32.,2.8));
#8580=CARTESIAN_POINT('',(1.15996323728161,32.4,6.5));
#8581=CARTESIAN_POINT('',(1.15996323728161,32.4,2.8));
#8582=CARTESIAN_POINT('Origin',(1.5,32.,6.5));
#8583=CARTESIAN_POINT('Origin',(0.,31.6,4.6));
#8584=CARTESIAN_POINT('',(2.2,31.6,2.8));
#8585=CARTESIAN_POINT('',(0.,31.6,2.8));
#8586=CARTESIAN_POINT('',(2.2,31.6,6.5));
#8587=CARTESIAN_POINT('',(2.2,31.6,2.7));
#8588=CARTESIAN_POINT('',(2.2,31.6,6.5));
#8589=CARTESIAN_POINT('Origin',(0.,31.6,4.6));
#8590=CARTESIAN_POINT('',(-1.15996323728161,31.6,6.5));
#8591=CARTESIAN_POINT('',(2.2,31.6,6.5));
#8592=CARTESIAN_POINT('',(-1.15996323728161,31.6,2.8));
#8593=CARTESIAN_POINT('',(-1.15996323728161,31.6,2.8));
#8594=CARTESIAN_POINT('',(0.,31.6,2.8));
#8595=CARTESIAN_POINT('',(-0.505,31.6,4.5));
#8596=CARTESIAN_POINT('Origin',(0.,31.6,4.5));
#8597=CARTESIAN_POINT('Origin',(-2.2,31.6,6.5));
#8598=CARTESIAN_POINT('',(2.2,32.4,6.5));
#8599=CARTESIAN_POINT('',(2.2,31.6,6.5));
#8600=CARTESIAN_POINT('',(2.2,32.4,6.5));
#8601=CARTESIAN_POINT('Origin',(-2.2,31.6,6.5));
#8602=CARTESIAN_POINT('',(-1.15996323728161,32.4,6.5));
#8603=CARTESIAN_POINT('',(2.2,32.4,6.5));
#8604=CARTESIAN_POINT('Origin',(-1.5,32.,6.5));
#8605=CARTESIAN_POINT('Origin',(0.,32.4,4.6));
#8606=CARTESIAN_POINT('',(2.2,32.4,2.8));
#8607=CARTESIAN_POINT('',(2.2,32.4,2.7));
#8608=CARTESIAN_POINT('',(0.,32.4,2.8));
#8609=CARTESIAN_POINT('Origin',(0.,32.4,4.6));
#8610=CARTESIAN_POINT('',(-1.15996323728161,32.4,2.8));
#8611=CARTESIAN_POINT('',(0.,32.4,2.8));
#8612=CARTESIAN_POINT('',(-1.15996323728161,32.4,2.8));
#8613=CARTESIAN_POINT('',(-0.505,32.4,4.5));
#8614=CARTESIAN_POINT('Origin',(0.,32.4,4.5));
#8615=CARTESIAN_POINT('Origin',(1.5,32.,1.9));
#8616=CARTESIAN_POINT('',(1.225,32.,2.));
#8617=CARTESIAN_POINT('Origin',(1.5,32.,2.));
#8618=CARTESIAN_POINT('',(1.225,32.,2.8));
#8619=CARTESIAN_POINT('',(1.225,32.,1.9));
#8620=CARTESIAN_POINT('Origin',(1.5,32.,2.8));
#8621=CARTESIAN_POINT('Origin',(-1.5,32.,2.8));
#8622=CARTESIAN_POINT('',(-1.84003676271839,32.4,6.5));
#8623=CARTESIAN_POINT('',(-1.84003676271839,32.4,2.8));
#8624=CARTESIAN_POINT('',(-1.84003676271839,32.4,2.8));
#8625=CARTESIAN_POINT('',(-1.84003676271839,31.6,6.5));
#8626=CARTESIAN_POINT('Origin',(-1.5,32.,6.5));
#8627=CARTESIAN_POINT('',(-1.84003676271839,31.6,2.8));
#8628=CARTESIAN_POINT('',(-1.84003676271839,31.6,2.8));
#8629=CARTESIAN_POINT('Origin',(-1.5,32.,2.8));
#8630=CARTESIAN_POINT('Origin',(-1.5,32.,2.8));
#8631=CARTESIAN_POINT('Origin',(-1.5,32.,2.8));
#8632=CARTESIAN_POINT('Origin',(0.,32.4,4.6));
#8633=CARTESIAN_POINT('',(-2.2,32.4,2.8));
#8634=CARTESIAN_POINT('',(0.,32.4,2.8));
#8635=CARTESIAN_POINT('',(-2.2,32.4,6.5));
#8636=CARTESIAN_POINT('',(-2.2,32.4,6.5));
#8637=CARTESIAN_POINT('',(2.2,32.4,6.5));
#8638=CARTESIAN_POINT('Origin',(-2.2,31.6,6.5));
#8639=CARTESIAN_POINT('',(-2.2,31.6,6.5));
#8640=CARTESIAN_POINT('',(-2.2,31.6,6.5));
#8641=CARTESIAN_POINT('',(2.2,31.6,6.5));
#8642=CARTESIAN_POINT('Origin',(0.,31.6,4.6));
#8643=CARTESIAN_POINT('',(-2.2,31.6,2.8));
#8644=CARTESIAN_POINT('',(-2.2,31.6,6.5));
#8645=CARTESIAN_POINT('',(0.,31.6,2.8));
#8646=CARTESIAN_POINT('Origin',(-1.5,32.,1.9));
#8647=CARTESIAN_POINT('',(-1.775,32.,2.));
#8648=CARTESIAN_POINT('Origin',(-1.5,32.,2.));
#8649=CARTESIAN_POINT('',(-1.775,32.,2.8));
#8650=CARTESIAN_POINT('',(-1.775,32.,1.9));
#8651=CARTESIAN_POINT('Origin',(-1.5,32.,2.8));
#8652=CARTESIAN_POINT('Origin',(0.,31.5,4.5));
#8653=CARTESIAN_POINT('',(-0.505,31.5,4.5));
#8654=CARTESIAN_POINT('Origin',(2.2,31.6,6.5));
#8655=CARTESIAN_POINT('',(2.2,31.8,2.8));
#8656=CARTESIAN_POINT('Origin',(-2.2,31.6,2.7));
#8657=CARTESIAN_POINT('',(-2.2,31.8,2.8));
#8658=CARTESIAN_POINT('Origin',(3.,33.2,2.));
#8659=CARTESIAN_POINT('',(3.,33.2,2.));
#8660=CARTESIAN_POINT('',(-3.,33.2,2.));
#8661=CARTESIAN_POINT('',(3.,33.2,2.));
#8662=CARTESIAN_POINT('',(-3.,33.2,2.8));
#8663=CARTESIAN_POINT('',(-3.,33.2,2.));
#8664=CARTESIAN_POINT('',(3.,33.2,2.8));
#8665=CARTESIAN_POINT('',(3.,33.2,2.8));
#8666=CARTESIAN_POINT('',(3.,33.2,2.));
#8667=CARTESIAN_POINT('Origin',(3.,30.8,2.));
#8668=CARTESIAN_POINT('',(3.,30.8,2.));
#8669=CARTESIAN_POINT('',(3.,30.8,2.));
#8670=CARTESIAN_POINT('',(3.,30.8,2.8));
#8671=CARTESIAN_POINT('',(3.,30.8,2.8));
#8672=CARTESIAN_POINT('',(3.,30.8,2.));
#8673=CARTESIAN_POINT('Origin',(-3.,30.8,2.));
#8674=CARTESIAN_POINT('',(-3.,30.8,2.));
#8675=CARTESIAN_POINT('',(-3.,30.8,2.));
#8676=CARTESIAN_POINT('',(-3.,30.8,2.8));
#8677=CARTESIAN_POINT('',(-3.,30.8,2.8));
#8678=CARTESIAN_POINT('',(-3.,30.8,2.));
#8679=CARTESIAN_POINT('Origin',(-3.,33.2,2.));
#8680=CARTESIAN_POINT('',(-3.,33.2,2.));
#8681=CARTESIAN_POINT('',(-3.,33.2,2.8));
#8682=CARTESIAN_POINT('Origin',(0.,32.,2.8));
#8683=CARTESIAN_POINT('Origin',(0.,32.,2.));
#8684=CARTESIAN_POINT('',(0.,0.,0.));
#8685=CARTESIAN_POINT('Origin',(-3.5,32.,1.9));
#8686=CARTESIAN_POINT('',(-3.775,32.,2.));
#8687=CARTESIAN_POINT('Origin',(-3.5,32.,2.));
#8688=CARTESIAN_POINT('',(-3.775,32.,2.8));
#8689=CARTESIAN_POINT('',(-3.775,32.,1.9));
#8690=CARTESIAN_POINT('Origin',(-3.5,32.,2.8));
#8691=CARTESIAN_POINT('Origin',(-5.1,32.,4.5));
#8692=CARTESIAN_POINT('',(-5.,32.,4.84));
#8693=CARTESIAN_POINT('Origin',(-5.,32.,4.5));
#8694=CARTESIAN_POINT('',(-4.2,32.,4.84));
#8695=CARTESIAN_POINT('',(-5.1,32.,4.84));
#8696=CARTESIAN_POINT('Origin',(-4.2,32.,4.5));
#8697=CARTESIAN_POINT('Origin',(-5.,33.2,5.5));
#8698=CARTESIAN_POINT('',(-5.,33.2,5.5));
#8699=CARTESIAN_POINT('',(-5.,30.8,5.5));
#8700=CARTESIAN_POINT('',(-5.,33.2,5.5));
#8701=CARTESIAN_POINT('',(-4.2,30.8,5.5));
#8702=CARTESIAN_POINT('',(-5.,30.8,5.5));
#8703=CARTESIAN_POINT('',(-4.2,33.2,5.5));
#8704=CARTESIAN_POINT('',(-4.2,33.2,5.5));
#8705=CARTESIAN_POINT('',(-5.,33.2,5.5));
#8706=CARTESIAN_POINT('Origin',(-4.2,32.,4.1));
#8707=CARTESIAN_POINT('',(-4.2,33.2,2.8));
#8708=CARTESIAN_POINT('',(-4.2,30.8,2.8));
#8709=CARTESIAN_POINT('',(-4.2,32.,2.8));
#8710=CARTESIAN_POINT('',(-4.2,33.2,2.7));
#8711=CARTESIAN_POINT('',(-4.2,30.8,5.5));
#8712=CARTESIAN_POINT('Origin',(-4.,32.,2.8));
#8713=CARTESIAN_POINT('',(-3.,30.8,2.8));
#8714=CARTESIAN_POINT('',(-5.,30.8,2.8));
#8715=CARTESIAN_POINT('',(-3.,33.2,2.8));
#8716=CARTESIAN_POINT('',(-3.,30.8,2.8));
#8717=CARTESIAN_POINT('',(-3.,33.2,2.8));
#8718=CARTESIAN_POINT('Origin',(-5.,30.8,2.));
#8719=CARTESIAN_POINT('',(-5.,30.8,2.));
#8720=CARTESIAN_POINT('',(-5.,30.8,2.));
#8721=CARTESIAN_POINT('',(-3.,30.8,2.));
#8722=CARTESIAN_POINT('',(-5.,30.8,2.));
#8723=CARTESIAN_POINT('',(-3.,30.8,2.));
#8724=CARTESIAN_POINT('Origin',(-3.,33.2,2.));
#8725=CARTESIAN_POINT('',(-3.,33.2,2.));
#8726=CARTESIAN_POINT('',(-3.,33.2,2.));
#8727=CARTESIAN_POINT('',(-5.,33.2,2.));
#8728=CARTESIAN_POINT('',(-3.,33.2,2.));
#8729=CARTESIAN_POINT('',(-5.,33.2,2.));
#8730=CARTESIAN_POINT('Origin',(-3.,30.8,2.));
#8731=CARTESIAN_POINT('',(-3.,30.8,2.));
#8732=CARTESIAN_POINT('Origin',(-5.,33.2,2.));
#8733=CARTESIAN_POINT('',(-5.,33.2,2.));
#8734=CARTESIAN_POINT('Origin',(-4.,32.,2.));
#8735=CARTESIAN_POINT('',(0.,0.,0.));
#8736=CARTESIAN_POINT('Origin',(-0.1,0.82,-0.3));
#8737=CARTESIAN_POINT('',(0.,0.82,-0.3));
#8738=CARTESIAN_POINT('',(0.,1.,-0.3));
#8739=CARTESIAN_POINT('',(0.,0.41,-0.3));
#8740=CARTESIAN_POINT('',(10.,0.82,-0.3));
#8741=CARTESIAN_POINT('',(-0.1,0.82,-0.3));
#8742=CARTESIAN_POINT('',(10.,1.,-0.3));
#8743=CARTESIAN_POINT('',(10.,0.41,-0.3));
#8744=CARTESIAN_POINT('',(-0.05,1.,-0.3));
#8745=CARTESIAN_POINT('Origin',(-0.1,0.82,-0.55));
#8746=CARTESIAN_POINT('',(0.,0.82,-0.55));
#8747=CARTESIAN_POINT('',(0.,0.82,-0.275));
#8748=CARTESIAN_POINT('',(10.,0.82,-0.55));
#8749=CARTESIAN_POINT('',(-0.1,0.82,-0.55));
#8750=CARTESIAN_POINT('',(10.,0.82,-0.275));
#8751=CARTESIAN_POINT('Origin',(-0.1,0.67,-0.55));
#8752=CARTESIAN_POINT('',(0.,0.67,-0.55));
#8753=CARTESIAN_POINT('',(0.,0.335,-0.55));
#8754=CARTESIAN_POINT('',(10.,0.67,-0.55));
#8755=CARTESIAN_POINT('',(-0.1,0.67,-0.55));
#8756=CARTESIAN_POINT('',(10.,0.335,-0.55));
#8757=CARTESIAN_POINT('Origin',(-0.1,0.42,-0.3));
#8758=CARTESIAN_POINT('',(0.,0.42,-0.3));
#8759=CARTESIAN_POINT('',(0.,0.24,-0.12));
#8760=CARTESIAN_POINT('',(10.,0.42,-0.3));
#8761=CARTESIAN_POINT('',(-0.1,0.42,-0.3));
#8762=CARTESIAN_POINT('',(10.,0.24,-0.12));
#8763=CARTESIAN_POINT('Origin',(-0.1,0.42,0.3));
#8764=CARTESIAN_POINT('',(0.,0.42,0.3));
#8765=CARTESIAN_POINT('',(0.,0.42,0.15));
#8766=CARTESIAN_POINT('',(10.,0.42,0.3));
#8767=CARTESIAN_POINT('',(-0.1,0.42,0.3));
#8768=CARTESIAN_POINT('',(10.,0.42,0.15));
#8769=CARTESIAN_POINT('Origin',(-0.1,0.67,0.55));
#8770=CARTESIAN_POINT('',(0.,0.67,0.55));
#8771=CARTESIAN_POINT('',(6.93889390390723E-18,0.365,0.245));
#8772=CARTESIAN_POINT('',(10.,0.67,0.55));
#8773=CARTESIAN_POINT('',(-0.1,0.67,0.55));
#8774=CARTESIAN_POINT('',(10.,0.365,0.245));
#8775=CARTESIAN_POINT('Origin',(-0.1,0.82,0.55));
#8776=CARTESIAN_POINT('',(0.,0.82,0.55));
#8777=CARTESIAN_POINT('',(0.,0.41,0.55));
#8778=CARTESIAN_POINT('',(10.,0.82,0.55));
#8779=CARTESIAN_POINT('',(-0.1,0.82,0.55));
#8780=CARTESIAN_POINT('',(10.,0.41,0.55));
#8781=CARTESIAN_POINT('Origin',(-0.1,0.82,0.3));
#8782=CARTESIAN_POINT('',(0.,0.82,0.3));
#8783=CARTESIAN_POINT('',(0.,0.82,0.15));
#8784=CARTESIAN_POINT('',(10.,0.82,0.3));
#8785=CARTESIAN_POINT('',(-0.1,0.82,0.3));
#8786=CARTESIAN_POINT('',(10.,0.82,0.15));
#8787=CARTESIAN_POINT('Origin',(-0.1,1.05,0.3));
#8788=CARTESIAN_POINT('',(0.,1.,0.3));
#8789=CARTESIAN_POINT('',(0.,0.525,0.3));
#8790=CARTESIAN_POINT('',(10.,1.,0.3));
#8791=CARTESIAN_POINT('',(-0.05,1.,0.3));
#8792=CARTESIAN_POINT('',(10.,0.525,0.3));
#8793=CARTESIAN_POINT('Origin',(-0.1,-0.3,-0.82));
#8794=CARTESIAN_POINT('',(0.,-0.3,-0.82));
#8795=CARTESIAN_POINT('',(0.,-0.3,-1.));
#8796=CARTESIAN_POINT('',(0.,-0.3,-0.41));
#8797=CARTESIAN_POINT('',(10.,-0.3,-0.82));
#8798=CARTESIAN_POINT('',(-0.1,-0.3,-0.82));
#8799=CARTESIAN_POINT('',(10.,-0.3,-1.));
#8800=CARTESIAN_POINT('',(10.,-0.3,-0.41));
#8801=CARTESIAN_POINT('',(-0.05,-0.3,-1.));
#8802=CARTESIAN_POINT('Origin',(-0.1,-0.55,-0.82));
#8803=CARTESIAN_POINT('',(0.,-0.55,-0.82));
#8804=CARTESIAN_POINT('',(0.,-0.275,-0.82));
#8805=CARTESIAN_POINT('',(10.,-0.55,-0.82));
#8806=CARTESIAN_POINT('',(-0.1,-0.55,-0.82));
#8807=CARTESIAN_POINT('',(10.,-0.275,-0.82));
#8808=CARTESIAN_POINT('Origin',(-0.1,-0.55,-0.67));
#8809=CARTESIAN_POINT('',(0.,-0.55,-0.67));
#8810=CARTESIAN_POINT('',(0.,-0.55,-0.335));
#8811=CARTESIAN_POINT('',(10.,-0.55,-0.67));
#8812=CARTESIAN_POINT('',(-0.1,-0.55,-0.67));
#8813=CARTESIAN_POINT('',(10.,-0.55,-0.335));
#8814=CARTESIAN_POINT('Origin',(-0.1,-0.3,-0.42));
#8815=CARTESIAN_POINT('',(0.,-0.3,-0.42));
#8816=CARTESIAN_POINT('',(0.,-0.12,-0.24));
#8817=CARTESIAN_POINT('',(10.,-0.3,-0.42));
#8818=CARTESIAN_POINT('',(-0.1,-0.3,-0.42));
#8819=CARTESIAN_POINT('',(10.,-0.12,-0.24));
#8820=CARTESIAN_POINT('Origin',(-0.1,0.3,-0.42));
#8821=CARTESIAN_POINT('',(0.,0.3,-0.42));
#8822=CARTESIAN_POINT('',(0.,0.15,-0.42));
#8823=CARTESIAN_POINT('',(10.,0.3,-0.42));
#8824=CARTESIAN_POINT('',(-0.1,0.3,-0.42));
#8825=CARTESIAN_POINT('',(10.,0.15,-0.42));
#8826=CARTESIAN_POINT('Origin',(-0.1,0.55,-0.67));
#8827=CARTESIAN_POINT('',(0.,0.55,-0.67));
#8828=CARTESIAN_POINT('',(0.,0.245,-0.365));
#8829=CARTESIAN_POINT('',(10.,0.55,-0.67));
#8830=CARTESIAN_POINT('',(-0.1,0.55,-0.67));
#8831=CARTESIAN_POINT('',(10.,0.245,-0.365));
#8832=CARTESIAN_POINT('Origin',(-0.1,0.55,-0.82));
#8833=CARTESIAN_POINT('',(0.,0.55,-0.82));
#8834=CARTESIAN_POINT('',(0.,0.55,-0.41));
#8835=CARTESIAN_POINT('',(10.,0.55,-0.82));
#8836=CARTESIAN_POINT('',(-0.1,0.55,-0.82));
#8837=CARTESIAN_POINT('',(10.,0.55,-0.41));
#8838=CARTESIAN_POINT('Origin',(-0.1,0.3,-0.82));
#8839=CARTESIAN_POINT('',(0.,0.3,-0.82));
#8840=CARTESIAN_POINT('',(0.,0.15,-0.82));
#8841=CARTESIAN_POINT('',(10.,0.3,-0.82));
#8842=CARTESIAN_POINT('',(-0.1,0.3,-0.82));
#8843=CARTESIAN_POINT('',(10.,0.15,-0.82));
#8844=CARTESIAN_POINT('Origin',(-0.1,0.3,-1.05));
#8845=CARTESIAN_POINT('',(0.,0.3,-1.));
#8846=CARTESIAN_POINT('',(0.,0.3,-0.525));
#8847=CARTESIAN_POINT('',(10.,0.3,-1.));
#8848=CARTESIAN_POINT('',(-0.05,0.3,-1.));
#8849=CARTESIAN_POINT('',(10.,0.3,-0.525));
#8850=CARTESIAN_POINT('Origin',(-0.1,-0.82,0.3));
#8851=CARTESIAN_POINT('',(0.,-0.82,0.3));
#8852=CARTESIAN_POINT('',(0.,-1.,0.3));
#8853=CARTESIAN_POINT('',(0.,-0.41,0.3));
#8854=CARTESIAN_POINT('',(10.,-0.82,0.3));
#8855=CARTESIAN_POINT('',(-0.1,-0.82,0.3));
#8856=CARTESIAN_POINT('',(10.,-1.,0.3));
#8857=CARTESIAN_POINT('',(10.,-0.41,0.3));
#8858=CARTESIAN_POINT('',(-0.05,-1.,0.3));
#8859=CARTESIAN_POINT('Origin',(-0.1,-0.82,0.55));
#8860=CARTESIAN_POINT('',(0.,-0.82,0.55));
#8861=CARTESIAN_POINT('',(0.,-0.82,0.275));
#8862=CARTESIAN_POINT('',(10.,-0.82,0.55));
#8863=CARTESIAN_POINT('',(-0.1,-0.82,0.55));
#8864=CARTESIAN_POINT('',(10.,-0.82,0.275));
#8865=CARTESIAN_POINT('Origin',(-0.1,-0.67,0.55));
#8866=CARTESIAN_POINT('',(0.,-0.67,0.55));
#8867=CARTESIAN_POINT('',(0.,-0.335,0.55));
#8868=CARTESIAN_POINT('',(10.,-0.67,0.55));
#8869=CARTESIAN_POINT('',(-0.1,-0.67,0.55));
#8870=CARTESIAN_POINT('',(10.,-0.335,0.55));
#8871=CARTESIAN_POINT('Origin',(-0.1,-0.42,0.3));
#8872=CARTESIAN_POINT('',(0.,-0.42,0.3));
#8873=CARTESIAN_POINT('',(-6.93889390390723E-18,-0.24,0.12));
#8874=CARTESIAN_POINT('',(10.,-0.42,0.3));
#8875=CARTESIAN_POINT('',(-0.1,-0.42,0.3));
#8876=CARTESIAN_POINT('',(10.,-0.24,0.12));
#8877=CARTESIAN_POINT('Origin',(-0.1,-0.42,-0.3));
#8878=CARTESIAN_POINT('',(0.,-0.42,-0.3));
#8879=CARTESIAN_POINT('',(0.,-0.42,-0.15));
#8880=CARTESIAN_POINT('',(10.,-0.42,-0.3));
#8881=CARTESIAN_POINT('',(-0.1,-0.42,-0.3));
#8882=CARTESIAN_POINT('',(10.,-0.42,-0.15));
#8883=CARTESIAN_POINT('Origin',(-0.1,-0.67,-0.55));
#8884=CARTESIAN_POINT('',(0.,-0.67,-0.55));
#8885=CARTESIAN_POINT('',(0.,-0.365,-0.245));
#8886=CARTESIAN_POINT('',(10.,-0.67,-0.55));
#8887=CARTESIAN_POINT('',(-0.1,-0.67,-0.55));
#8888=CARTESIAN_POINT('',(10.,-0.365,-0.245));
#8889=CARTESIAN_POINT('Origin',(-0.1,-0.82,-0.55));
#8890=CARTESIAN_POINT('',(0.,-0.82,-0.55));
#8891=CARTESIAN_POINT('',(0.,-0.41,-0.55));
#8892=CARTESIAN_POINT('',(10.,-0.82,-0.55));
#8893=CARTESIAN_POINT('',(-0.1,-0.82,-0.55));
#8894=CARTESIAN_POINT('',(10.,-0.41,-0.55));
#8895=CARTESIAN_POINT('Origin',(-0.1,-0.82,-0.3));
#8896=CARTESIAN_POINT('',(0.,-0.82,-0.3));
#8897=CARTESIAN_POINT('',(0.,-0.82,-0.15));
#8898=CARTESIAN_POINT('',(10.,-0.82,-0.3));
#8899=CARTESIAN_POINT('',(-0.1,-0.82,-0.3));
#8900=CARTESIAN_POINT('',(10.,-0.82,-0.15));
#8901=CARTESIAN_POINT('Origin',(-0.1,-1.05,-0.3));
#8902=CARTESIAN_POINT('',(0.,-1.,-0.3));
#8903=CARTESIAN_POINT('',(0.,-0.525,-0.3));
#8904=CARTESIAN_POINT('',(10.,-1.,-0.3));
#8905=CARTESIAN_POINT('',(-0.05,-1.,-0.3));
#8906=CARTESIAN_POINT('',(10.,-0.525,-0.3));
#8907=CARTESIAN_POINT('Origin',(-0.1,0.3,0.82));
#8908=CARTESIAN_POINT('',(0.,0.3,0.82));
#8909=CARTESIAN_POINT('',(0.,0.3,1.));
#8910=CARTESIAN_POINT('',(0.,0.3,0.41));
#8911=CARTESIAN_POINT('',(10.,0.3,0.82));
#8912=CARTESIAN_POINT('',(-0.1,0.3,0.82));
#8913=CARTESIAN_POINT('',(10.,0.3,1.));
#8914=CARTESIAN_POINT('',(10.,0.3,0.41));
#8915=CARTESIAN_POINT('',(-0.05,0.3,1.));
#8916=CARTESIAN_POINT('Origin',(-0.1,0.55,0.82));
#8917=CARTESIAN_POINT('',(0.,0.55,0.82));
#8918=CARTESIAN_POINT('',(0.,0.275,0.82));
#8919=CARTESIAN_POINT('',(10.,0.55,0.82));
#8920=CARTESIAN_POINT('',(-0.1,0.55,0.82));
#8921=CARTESIAN_POINT('',(10.,0.275,0.82));
#8922=CARTESIAN_POINT('Origin',(-0.1,0.55,0.67));
#8923=CARTESIAN_POINT('',(0.,0.55,0.67));
#8924=CARTESIAN_POINT('',(0.,0.55,0.335));
#8925=CARTESIAN_POINT('',(10.,0.55,0.67));
#8926=CARTESIAN_POINT('',(-0.1,0.55,0.67));
#8927=CARTESIAN_POINT('',(10.,0.55,0.335));
#8928=CARTESIAN_POINT('Origin',(-0.1,0.3,0.42));
#8929=CARTESIAN_POINT('',(0.,0.3,0.42));
#8930=CARTESIAN_POINT('',(6.93889390390723E-18,0.12,0.24));
#8931=CARTESIAN_POINT('',(10.,0.3,0.42));
#8932=CARTESIAN_POINT('',(-0.1,0.3,0.42));
#8933=CARTESIAN_POINT('',(10.,0.12,0.24));
#8934=CARTESIAN_POINT('Origin',(-0.1,-0.3,0.42));
#8935=CARTESIAN_POINT('',(0.,-0.3,0.42));
#8936=CARTESIAN_POINT('',(0.,-0.15,0.42));
#8937=CARTESIAN_POINT('',(10.,-0.3,0.42));
#8938=CARTESIAN_POINT('',(-0.1,-0.3,0.42));
#8939=CARTESIAN_POINT('',(10.,-0.15,0.42));
#8940=CARTESIAN_POINT('Origin',(-0.1,-0.55,0.67));
#8941=CARTESIAN_POINT('',(0.,-0.55,0.67));
#8942=CARTESIAN_POINT('',(6.93889390390723E-18,-0.245,0.365));
#8943=CARTESIAN_POINT('',(10.,-0.55,0.67));
#8944=CARTESIAN_POINT('',(-0.1,-0.55,0.67));
#8945=CARTESIAN_POINT('',(10.,-0.245,0.365));
#8946=CARTESIAN_POINT('Origin',(-0.1,-0.55,0.82));
#8947=CARTESIAN_POINT('',(0.,-0.55,0.82));
#8948=CARTESIAN_POINT('',(0.,-0.55,0.41));
#8949=CARTESIAN_POINT('',(10.,-0.55,0.82));
#8950=CARTESIAN_POINT('',(-0.1,-0.55,0.82));
#8951=CARTESIAN_POINT('',(10.,-0.55,0.41));
#8952=CARTESIAN_POINT('Origin',(-0.1,-0.3,0.82));
#8953=CARTESIAN_POINT('',(0.,-0.3,0.82));
#8954=CARTESIAN_POINT('',(0.,-0.15,0.82));
#8955=CARTESIAN_POINT('',(10.,-0.3,0.82));
#8956=CARTESIAN_POINT('',(-0.1,-0.3,0.82));
#8957=CARTESIAN_POINT('',(10.,-0.15,0.82));
#8958=CARTESIAN_POINT('Origin',(-0.1,-0.3,1.05));
#8959=CARTESIAN_POINT('',(0.,-0.3,1.));
#8960=CARTESIAN_POINT('',(0.,-0.3,0.525));
#8961=CARTESIAN_POINT('',(10.,-0.3,1.));
#8962=CARTESIAN_POINT('',(-0.05,-0.3,1.));
#8963=CARTESIAN_POINT('',(10.,-0.3,0.525));
#8964=CARTESIAN_POINT('Origin',(-0.1,0.,0.));
#8965=CARTESIAN_POINT('',(0.,-2.57175827820944E-17,0.21));
#8966=CARTESIAN_POINT('Origin',(0.,0.,0.));
#8967=CARTESIAN_POINT('',(10.,2.57175827820944E-17,0.21));
#8968=CARTESIAN_POINT('',(-0.1,-2.57175827820944E-17,0.21));
#8969=CARTESIAN_POINT('Origin',(10.,0.,0.));
#8970=CARTESIAN_POINT('Origin',(0.,1.,-1.));
#8971=CARTESIAN_POINT('',(0.,1.,1.));
#8972=CARTESIAN_POINT('',(0.,1.,-1.));
#8973=CARTESIAN_POINT('',(10.,1.,1.));
#8974=CARTESIAN_POINT('',(0.,1.,1.));
#8975=CARTESIAN_POINT('',(10.,1.,-1.));
#8976=CARTESIAN_POINT('Origin',(0.,1.,-1.));
#8977=CARTESIAN_POINT('',(10.,1.,-1.));
#8978=CARTESIAN_POINT('',(10.,1.,-1.));
#8979=CARTESIAN_POINT('',(0.,1.,-1.));
#8980=CARTESIAN_POINT('',(0.,1.,-1.));
#8981=CARTESIAN_POINT('',(0.,1.,-1.));
#8982=CARTESIAN_POINT('Origin',(0.,-1.,-1.));
#8983=CARTESIAN_POINT('',(0.,-1.,-1.));
#8984=CARTESIAN_POINT('',(10.,-1.,-1.));
#8985=CARTESIAN_POINT('Origin',(0.,-1.,-1.));
#8986=CARTESIAN_POINT('',(10.,-1.,-1.));
#8987=CARTESIAN_POINT('',(10.,-1.,-1.));
#8988=CARTESIAN_POINT('',(0.,-1.,-1.));
#8989=CARTESIAN_POINT('',(0.,-1.,-1.));
#8990=CARTESIAN_POINT('',(0.,-1.,-1.));
#8991=CARTESIAN_POINT('Origin',(0.,-1.,1.));
#8992=CARTESIAN_POINT('',(0.,-1.,1.));
#8993=CARTESIAN_POINT('',(10.,-1.,1.));
#8994=CARTESIAN_POINT('Origin',(0.,-1.,1.));
#8995=CARTESIAN_POINT('',(10.,-1.,1.));
#8996=CARTESIAN_POINT('',(10.,-1.,1.));
#8997=CARTESIAN_POINT('',(0.,-1.,1.));
#8998=CARTESIAN_POINT('',(0.,-1.,1.));
#8999=CARTESIAN_POINT('',(0.,-1.,1.));
#9000=CARTESIAN_POINT('Origin',(0.,1.,1.));
#9001=CARTESIAN_POINT('',(0.,1.,1.));
#9002=CARTESIAN_POINT('',(10.,1.,1.));
#9003=CARTESIAN_POINT('Origin',(0.,1.,1.));
#9004=CARTESIAN_POINT('',(10.,1.,1.));
#9005=CARTESIAN_POINT('',(0.,1.,1.));
#9006=CARTESIAN_POINT('Origin',(10.,0.,0.));
#9007=CARTESIAN_POINT('Origin',(0.,0.,0.));
#9008=CARTESIAN_POINT('',(0.,0.,0.));
#9009=CARTESIAN_POINT('Origin',(-0.25,-0.225,0.075));
#9010=CARTESIAN_POINT('',(0.5,-0.15,0.));
#9011=CARTESIAN_POINT('',(0.5,-0.3,0.15));
#9012=CARTESIAN_POINT('',(0.5,-0.225,0.075));
#9013=CARTESIAN_POINT('',(-0.5,-0.3,0.15));
#9014=CARTESIAN_POINT('',(-0.25,-0.3,0.15));
#9015=CARTESIAN_POINT('',(-0.5,-0.15,0.));
#9016=CARTESIAN_POINT('',(-0.5,-0.075,-0.075));
#9017=CARTESIAN_POINT('',(-0.149388386429468,-0.15,0.));
#9018=CARTESIAN_POINT('',(-0.25,-0.15,0.));
#9019=CARTESIAN_POINT('',(0.149388386429468,-0.15,0.));
#9020=CARTESIAN_POINT('Origin',(0.,0.,-0.15));
#9021=CARTESIAN_POINT('',(-0.25,-0.15,0.));
#9022=CARTESIAN_POINT('Origin',(0.,0.,-0.1));
#9023=CARTESIAN_POINT('',(-0.2117,-2.59257727379495E-17,0.));
#9024=CARTESIAN_POINT('Origin',(0.,0.,0.));
#9025=CARTESIAN_POINT('',(-0.2117,2.59257727379495E-17,0.4));
#9026=CARTESIAN_POINT('',(-0.2117,-2.59257727379495E-17,-0.1));
#9027=CARTESIAN_POINT('Origin',(0.,0.,0.4));
#9028=CARTESIAN_POINT('',(-0.149388386429468,0.15,0.));
#9029=CARTESIAN_POINT('Origin',(0.,0.,0.));
#9030=CARTESIAN_POINT('',(0.149388386429468,0.15,0.));
#9031=CARTESIAN_POINT('Origin',(0.,0.,-0.15));
#9032=CARTESIAN_POINT('Origin',(0.,0.,0.));
#9033=CARTESIAN_POINT('Origin',(0.,0.,0.));
#9034=CARTESIAN_POINT('',(-0.5,0.15,0.));
#9035=CARTESIAN_POINT('',(-0.5,0.3,0.));
#9036=CARTESIAN_POINT('',(0.25,0.15,0.));
#9037=CARTESIAN_POINT('Origin',(0.,0.,0.));
#9038=CARTESIAN_POINT('',(0.5,0.15,0.));
#9039=CARTESIAN_POINT('',(0.25,0.15,0.));
#9040=CARTESIAN_POINT('',(0.5,-0.3,0.));
#9041=CARTESIAN_POINT('Origin',(0.25,0.225,0.075));
#9042=CARTESIAN_POINT('',(-0.5,0.3,0.15));
#9043=CARTESIAN_POINT('',(-0.5,0.225,0.075));
#9044=CARTESIAN_POINT('',(0.5,0.3,0.15));
#9045=CARTESIAN_POINT('',(0.25,0.3,0.15));
#9046=CARTESIAN_POINT('',(0.5,0.075,-0.075));
#9047=CARTESIAN_POINT('Origin',(0.5,-0.3,0.));
#9048=CARTESIAN_POINT('',(0.5,0.3,0.4));
#9049=CARTESIAN_POINT('',(0.5,0.3,0.));
#9050=CARTESIAN_POINT('',(0.5,-0.3,0.4));
#9051=CARTESIAN_POINT('',(0.5,-0.3,0.4));
#9052=CARTESIAN_POINT('',(0.5,-0.3,0.));
#9053=CARTESIAN_POINT('Origin',(0.5,0.3,0.));
#9054=CARTESIAN_POINT('',(-0.5,0.3,0.4));
#9055=CARTESIAN_POINT('',(-0.5,0.3,0.));
#9056=CARTESIAN_POINT('',(0.5,0.3,0.4));
#9057=CARTESIAN_POINT('Origin',(-0.5,-0.3,0.));
#9058=CARTESIAN_POINT('',(-0.5,-0.3,0.4));
#9059=CARTESIAN_POINT('',(-0.5,-0.3,0.4));
#9060=CARTESIAN_POINT('',(-0.5,-0.3,0.));
#9061=CARTESIAN_POINT('Origin',(-0.5,0.3,0.));
#9062=CARTESIAN_POINT('',(-0.5,0.3,0.4));
#9063=CARTESIAN_POINT('Origin',(0.,0.,0.4));
#9064=CARTESIAN_POINT('',(0.,0.,0.));
#9065=CARTESIAN_POINT('Origin',(0.,0.09,0.));
#9066=CARTESIAN_POINT('',(-0.285,0.1,3.49024337756996E-17));
#9067=CARTESIAN_POINT('Origin',(0.,0.1,0.));
#9068=CARTESIAN_POINT('',(-0.265,0.08,-3.24531401774049E-17));
#9069=CARTESIAN_POINT('',(-0.275,0.09,3.36777869765522E-17));
#9070=CARTESIAN_POINT('Origin',(0.,0.08,0.));
#9071=CARTESIAN_POINT('Origin',(0.,0.,0.));
#9072=CARTESIAN_POINT('',(-0.265,0.,3.24531401774049E-17));
#9073=CARTESIAN_POINT('',(-0.265,0.,3.24531401774049E-17));
#9074=CARTESIAN_POINT('Origin',(0.,0.,0.));
#9075=CARTESIAN_POINT('Origin',(0.,0.1,0.));
#9076=CARTESIAN_POINT('',(-0.5,0.1,6.12323399573677E-17));
#9077=CARTESIAN_POINT('Origin',(0.,0.1,0.));
#9078=CARTESIAN_POINT('Origin',(0.,0.,0.));
#9079=CARTESIAN_POINT('',(-0.5,0.,6.12323399573677E-17));
#9080=CARTESIAN_POINT('',(-0.5,0.,6.12323399573677E-17));
#9081=CARTESIAN_POINT('Origin',(0.,0.,0.));
#9082=CARTESIAN_POINT('Origin',(0.,0.,0.));
#9083=CARTESIAN_POINT('',(0.,0.,0.));
#9084=CARTESIAN_POINT('Origin',(0.115470053837925,-0.5,-0.2));
#9085=CARTESIAN_POINT('',(0.23094010767585,-0.5,0.));
#9086=CARTESIAN_POINT('',(0.115470053837925,-0.5,-0.2));
#9087=CARTESIAN_POINT('',(0.23094010767585,-0.5,0.));
#9088=CARTESIAN_POINT('',(0.115470053837925,-0.8,-0.2));
#9089=CARTESIAN_POINT('',(0.115470053837925,-0.5,-0.2));
#9090=CARTESIAN_POINT('',(0.23094010767585,-0.8,0.));
#9091=CARTESIAN_POINT('',(0.23094010767585,-0.8,0.));
#9092=CARTESIAN_POINT('',(0.23094010767585,-0.5,0.));
#9093=CARTESIAN_POINT('Origin',(-0.115470053837925,-0.5,-0.2));
#9094=CARTESIAN_POINT('',(-0.115470053837925,-0.5,-0.2));
#9095=CARTESIAN_POINT('',(0.115470053837925,-0.5,-0.2));
#9096=CARTESIAN_POINT('',(-0.115470053837925,-0.8,-0.2));
#9097=CARTESIAN_POINT('',(-0.115470053837925,-0.5,-0.2));
#9098=CARTESIAN_POINT('',(0.115470053837925,-0.8,-0.2));
#9099=CARTESIAN_POINT('Origin',(-0.23094010767585,-0.5,-2.77555756156289E-17));
#9100=CARTESIAN_POINT('',(-0.23094010767585,-0.5,-2.82820063659975E-17));
#9101=CARTESIAN_POINT('',(-0.115470053837925,-0.5,-0.2));
#9102=CARTESIAN_POINT('',(-0.23094010767585,-0.8,-2.77555756156289E-17));
#9103=CARTESIAN_POINT('',(-0.23094010767585,-0.5,-2.82820063659975E-17));
#9104=CARTESIAN_POINT('',(-0.115470053837925,-0.8,-0.2));
#9105=CARTESIAN_POINT('Origin',(-0.115470053837925,-0.5,0.2));
#9106=CARTESIAN_POINT('',(-0.115470053837925,-0.5,0.2));
#9107=CARTESIAN_POINT('',(-0.23094010767585,-0.5,-2.82820063659975E-17));
#9108=CARTESIAN_POINT('',(-0.115470053837925,-0.8,0.2));
#9109=CARTESIAN_POINT('',(-0.115470053837925,-0.5,0.2));
#9110=CARTESIAN_POINT('',(-0.23094010767585,-0.8,-2.82820063659975E-17));
#9111=CARTESIAN_POINT('Origin',(0.115470053837925,-0.5,0.2));
#9112=CARTESIAN_POINT('',(0.115470053837925,-0.5,0.2));
#9113=CARTESIAN_POINT('',(-0.115470053837925,-0.5,0.2));
#9114=CARTESIAN_POINT('',(0.115470053837925,-0.8,0.2));
#9115=CARTESIAN_POINT('',(0.115470053837925,-0.5,0.2));
#9116=CARTESIAN_POINT('',(-0.115470053837925,-0.8,0.2));
#9117=CARTESIAN_POINT('Origin',(0.23094010767585,-0.5,0.));
#9118=CARTESIAN_POINT('',(0.115470053837925,-0.5,0.2));
#9119=CARTESIAN_POINT('',(0.115470053837925,-0.8,0.2));
#9120=CARTESIAN_POINT('Origin',(0.,-0.5,0.));
#9121=CARTESIAN_POINT('Origin',(0.,-0.8,0.));
#9122=CARTESIAN_POINT('Origin',(0.,-1.4,0.));
#9123=CARTESIAN_POINT('',(-0.24505,-1.4,3.00099698131059E-17));
#9124=CARTESIAN_POINT('Origin',(0.,-1.4,0.));
#9125=CARTESIAN_POINT('Origin',(0.375,0.5,0.));
#9126=CARTESIAN_POINT('',(-0.375,0.5,-4.59242549680257E-17));
#9127=CARTESIAN_POINT('Origin',(0.,0.5,0.));
#9128=CARTESIAN_POINT('Origin',(0.,0.475,0.));
#9129=CARTESIAN_POINT('',(-0.425,0.45,-5.20474889637625E-17));
#9130=CARTESIAN_POINT('Origin',(0.,0.45,0.));
#9131=CARTESIAN_POINT('',(-0.4,0.475,-4.89858719658941E-17));
#9132=CARTESIAN_POINT('Origin',(0.,0.24,0.));
#9133=CARTESIAN_POINT('',(-0.425,0.0299999999999998,-5.20474889637625E-17));
#9134=CARTESIAN_POINT('Origin',(0.,0.0299999999999998,0.));
#9135=CARTESIAN_POINT('',(-0.425,0.24,-5.20474889637625E-17));
#9136=CARTESIAN_POINT('Origin',(0.,0.0150000000000001,0.));
#9137=CARTESIAN_POINT('',(-0.395,4.85722573273506E-17,-4.83735485663204E-17));
#9138=CARTESIAN_POINT('Origin',(0.,0.,0.));
#9139=CARTESIAN_POINT('',(-0.41,0.0150000000000001,-5.02105187650415E-17));
#9140=CARTESIAN_POINT('Origin',(0.27,0.,0.));
#9141=CARTESIAN_POINT('',(-0.27,0.,-3.30654635769785E-17));
#9142=CARTESIAN_POINT('Origin',(0.,0.,0.));
#9143=CARTESIAN_POINT('Origin',(0.,-0.02,0.));
#9144=CARTESIAN_POINT('',(-0.24505,-0.0498999999999999,3.00099698131059E-17));
#9145=CARTESIAN_POINT('Origin',(0.,-0.0498999999999999,0.));
#9146=CARTESIAN_POINT('',(-0.26,-0.02,-3.18408167778312E-17));
#9147=CARTESIAN_POINT('Origin',(0.,-0.995,0.));
#9148=CARTESIAN_POINT('',(-0.24505,-0.995,-3.00099698131059E-17));
#9149=CARTESIAN_POINT('',(0.,0.,0.));
#9150=CARTESIAN_POINT('Origin',(0.,-1.935,0.));
#9151=CARTESIAN_POINT('',(-0.3933,-3.9267,4.81653586104654E-17));
#9152=CARTESIAN_POINT('Origin',(0.,-3.9267,0.));
#9153=CARTESIAN_POINT('',(-0.3933,0.,-4.81653586104654E-17));
#9154=CARTESIAN_POINT('',(-0.3933,-1.935,-4.81653586104654E-17));
#9155=CARTESIAN_POINT('Origin',(0.,0.,0.));
#9156=CARTESIAN_POINT('Origin',(0.,-3.96,0.));
#9157=CARTESIAN_POINT('',(-0.32,-4.,-3.91886975727153E-17));
#9158=CARTESIAN_POINT('Origin',(0.,-4.,0.));
#9159=CARTESIAN_POINT('',(-0.36,-3.96,-4.40872847693047E-17));
#9160=CARTESIAN_POINT('Origin',(0.,-4.,0.));
#9161=CARTESIAN_POINT('Origin',(0.,0.462722715486149,0.));
#9162=CARTESIAN_POINT('',(-0.6175,0.53,-7.5621939847349E-17));
#9163=CARTESIAN_POINT('Origin',(0.,0.53,0.));
#9164=CARTESIAN_POINT('',(-0.750555349946514,0.453180457891261,-9.19165206894919E-17));
#9165=CARTESIAN_POINT('',(-0.734027674973257,0.462722715486149,-8.98924642641573E-17));
#9166=CARTESIAN_POINT('',(-0.375277674973257,0.453180457891261,0.65));
#9167=CARTESIAN_POINT('Ctrl Pts',(-0.375277674973257,0.45318045789126,0.65));
#9168=CARTESIAN_POINT('Ctrl Pts',(-0.562916512459968,0.561513791224244,
0.324999999999856));
#9169=CARTESIAN_POINT('Ctrl Pts',(-0.750555349946514,0.45318045789126,-9.19165206894919E-17));
#9170=CARTESIAN_POINT('',(0.375277674973257,0.453180457891261,0.65));
#9171=CARTESIAN_POINT('Ctrl Pts',(0.375277674973257,0.453180457891261,0.65));
#9172=CARTESIAN_POINT('Ctrl Pts',(-1.66922031752392E-13,0.561513791224244,
0.65));
#9173=CARTESIAN_POINT('Ctrl Pts',(-0.375277674973257,0.45318045789126,0.65));
#9174=CARTESIAN_POINT('',(0.750555349946514,0.453180457891261,0.));
#9175=CARTESIAN_POINT('Ctrl Pts',(0.750555349946514,0.453180457891261,0.));
#9176=CARTESIAN_POINT('Ctrl Pts',(0.562916512459802,0.561513791224244,0.325000000000144));
#9177=CARTESIAN_POINT('Ctrl Pts',(0.375277674973257,0.45318045789126,0.65));
#9178=CARTESIAN_POINT('',(0.375277674973257,0.453180457891261,-0.65));
#9179=CARTESIAN_POINT('Ctrl Pts',(0.375277674973257,0.45318045789126,-0.65));
#9180=CARTESIAN_POINT('Ctrl Pts',(0.562916512459968,0.561513791224244,-0.324999999999855));
#9181=CARTESIAN_POINT('Ctrl Pts',(0.750555349946514,0.453180457891261,0.));
#9182=CARTESIAN_POINT('',(-0.375277674973257,0.45318045789126,-0.65));
#9183=CARTESIAN_POINT('Ctrl Pts',(-0.375277674973257,0.453180457891261,
-0.65));
#9184=CARTESIAN_POINT('Ctrl Pts',(1.66866520601161E-13,0.561513791224244,
-0.65));
#9185=CARTESIAN_POINT('Ctrl Pts',(0.375277674973257,0.45318045789126,-0.65));
#9186=CARTESIAN_POINT('Ctrl Pts',(-0.750555349946514,0.453180457891261,
-9.19165206894919E-17));
#9187=CARTESIAN_POINT('Ctrl Pts',(-0.562916512459802,0.561513791224244,
-0.325000000000144));
#9188=CARTESIAN_POINT('Ctrl Pts',(-0.375277674973257,0.45318045789126,-0.65));
#9189=CARTESIAN_POINT('Origin',(0.375277674973257,0.,-0.65));
#9190=CARTESIAN_POINT('',(0.375277674973257,0.,-0.65));
#9191=CARTESIAN_POINT('',(0.375277674973257,0.,-0.65));
#9192=CARTESIAN_POINT('',(-0.375277674973257,0.,-0.65));
#9193=CARTESIAN_POINT('',(0.375277674973257,0.,-0.65));
#9194=CARTESIAN_POINT('',(-0.375277674973257,0.,-0.65));
#9195=CARTESIAN_POINT('Origin',(0.750555349946514,0.,0.));
#9196=CARTESIAN_POINT('',(0.750555349946514,0.,0.));
#9197=CARTESIAN_POINT('',(0.750555349946514,0.,0.));
#9198=CARTESIAN_POINT('',(0.750555349946514,0.,0.));
#9199=CARTESIAN_POINT('Origin',(0.375277674973257,0.,0.65));
#9200=CARTESIAN_POINT('',(0.375277674973257,0.,0.65));
#9201=CARTESIAN_POINT('',(0.375277674973257,0.,0.65));
#9202=CARTESIAN_POINT('',(0.375277674973257,0.,0.65));
#9203=CARTESIAN_POINT('Origin',(-0.375277674973257,0.,0.65));
#9204=CARTESIAN_POINT('',(-0.375277674973257,0.,0.65));
#9205=CARTESIAN_POINT('',(-0.375277674973257,0.,0.65));
#9206=CARTESIAN_POINT('',(-0.375277674973257,0.,0.65));
#9207=CARTESIAN_POINT('Origin',(-0.750555349946514,0.,-9.19165206894919E-17));
#9208=CARTESIAN_POINT('',(-0.750555349946514,0.,-9.19165206894919E-17));
#9209=CARTESIAN_POINT('',(-0.750555349946514,0.,-9.19165206894919E-17));
#9210=CARTESIAN_POINT('',(-0.750555349946514,0.,-9.19165206894919E-17));
#9211=CARTESIAN_POINT('Origin',(-0.375277674973257,0.,-0.65));
#9212=CARTESIAN_POINT('',(-0.375277674973257,0.,-0.65));
#9213=CARTESIAN_POINT('Origin',(0.,0.53,-1.11022302462516E-16));
#9214=CARTESIAN_POINT('Origin',(0.,0.,-1.11022302462516E-16));
#9215=CARTESIAN_POINT('',(0.,0.,0.));
#9216=CARTESIAN_POINT('Origin',(0.,0.067277284513851,0.));
#9217=CARTESIAN_POINT('',(-0.375277674973257,0.0768195421087395,0.65));
#9218=CARTESIAN_POINT('',(0.375277674973257,0.0768195421087395,0.65));
#9219=CARTESIAN_POINT('Ctrl Pts',(-0.375277674973257,0.0768195421087395,
0.65));
#9220=CARTESIAN_POINT('Ctrl Pts',(1.66533453693773E-13,-0.0315137912242439,
0.65));
#9221=CARTESIAN_POINT('Ctrl Pts',(0.375277674973257,0.0768195421087394,
0.65));
#9222=CARTESIAN_POINT('',(-0.750555349946514,0.0768195421087394,-9.19165206894919E-17));
#9223=CARTESIAN_POINT('Ctrl Pts',(-0.750555349946514,0.0768195421087394,
-9.19165206894919E-17));
#9224=CARTESIAN_POINT('Ctrl Pts',(-0.562916512459802,-0.0315137912242434,
0.325000000000144));
#9225=CARTESIAN_POINT('Ctrl Pts',(-0.375277674973257,0.0768195421087395,
0.65));
#9226=CARTESIAN_POINT('',(-0.6175,-2.77555756156289E-17,-7.5621939847349E-17));
#9227=CARTESIAN_POINT('',(-0.734027674973257,0.067277284513851,-8.98924642641573E-17));
#9228=CARTESIAN_POINT('Origin',(0.,0.,0.));
#9229=CARTESIAN_POINT('',(-0.375277674973257,0.0768195421087395,-0.65));
#9230=CARTESIAN_POINT('Ctrl Pts',(-0.375277674973257,0.0768195421087395,
-0.65));
#9231=CARTESIAN_POINT('Ctrl Pts',(-0.562916512459968,-0.0315137912242437,
-0.324999999999856));
#9232=CARTESIAN_POINT('Ctrl Pts',(-0.750555349946514,0.0768195421087395,
-9.19165206894919E-17));
#9233=CARTESIAN_POINT('',(0.375277674973257,0.0768195421087395,-0.65));
#9234=CARTESIAN_POINT('Ctrl Pts',(0.375277674973257,0.0768195421087395,
-0.65));
#9235=CARTESIAN_POINT('Ctrl Pts',(-1.66144875635155E-13,-0.0315137912242437,
-0.65));
#9236=CARTESIAN_POINT('Ctrl Pts',(-0.375277674973257,0.0768195421087395,
-0.65));
#9237=CARTESIAN_POINT('',(0.750555349946514,0.0768195421087394,0.));
#9238=CARTESIAN_POINT('Ctrl Pts',(0.750555349946514,0.0768195421087394,
0.));
#9239=CARTESIAN_POINT('Ctrl Pts',(0.562916512459802,-0.0315137912242436,
-0.325000000000144));
#9240=CARTESIAN_POINT('Ctrl Pts',(0.375277674973257,0.0768195421087395,
-0.65));
#9241=CARTESIAN_POINT('Ctrl Pts',(0.375277674973257,0.0768195421087394,
0.65));
#9242=CARTESIAN_POINT('Ctrl Pts',(0.562916512459968,-0.0315137912242439,
0.324999999999856));
#9243=CARTESIAN_POINT('Ctrl Pts',(0.750555349946514,0.0768195421087394,
0.));
#9244=CARTESIAN_POINT('Origin',(0.,0.612722715486149,0.));
#9245=CARTESIAN_POINT('',(-0.6175,0.68,-7.5621939847349E-17));
#9246=CARTESIAN_POINT('Origin',(0.,0.68,0.));
#9247=CARTESIAN_POINT('',(-0.750555349946514,0.603180457891261,-9.19165206894919E-17));
#9248=CARTESIAN_POINT('',(-0.734027674973257,0.612722715486149,-8.98924642641573E-17));
#9249=CARTESIAN_POINT('',(-0.375277674973257,0.603180457891261,0.65));
#9250=CARTESIAN_POINT('Ctrl Pts',(-0.375277674973257,0.603180457891261,
0.65));
#9251=CARTESIAN_POINT('Ctrl Pts',(-0.562916512459968,0.711513791224243,
0.324999999999856));
#9252=CARTESIAN_POINT('Ctrl Pts',(-0.750555349946514,0.603180457891261,
-9.19165206894919E-17));
#9253=CARTESIAN_POINT('',(0.375277674973257,0.603180457891261,0.65));
#9254=CARTESIAN_POINT('Ctrl Pts',(0.375277674973257,0.603180457891261,0.65));
#9255=CARTESIAN_POINT('Ctrl Pts',(-1.66755498298699E-13,0.711513791224244,
0.65));
#9256=CARTESIAN_POINT('Ctrl Pts',(-0.375277674973257,0.603180457891261,
0.65));
#9257=CARTESIAN_POINT('',(0.750555349946514,0.603180457891261,0.));
#9258=CARTESIAN_POINT('Ctrl Pts',(0.750555349946514,0.603180457891261,0.));
#9259=CARTESIAN_POINT('Ctrl Pts',(0.562916512459802,0.711513791224244,0.325000000000144));
#9260=CARTESIAN_POINT('Ctrl Pts',(0.375277674973257,0.603180457891261,0.65));
#9261=CARTESIAN_POINT('',(0.375277674973257,0.603180457891261,-0.65));
#9262=CARTESIAN_POINT('Ctrl Pts',(0.375277674973257,0.603180457891261,-0.65));
#9263=CARTESIAN_POINT('Ctrl Pts',(0.562916512459969,0.711513791224244,-0.324999999999856));
#9264=CARTESIAN_POINT('Ctrl Pts',(0.750555349946514,0.603180457891261,0.));
#9265=CARTESIAN_POINT('',(-0.375277674973257,0.603180457891261,-0.65));
#9266=CARTESIAN_POINT('Ctrl Pts',(-0.375277674973257,0.603180457891261,
-0.65));
#9267=CARTESIAN_POINT('Ctrl Pts',(1.66422431391311E-13,0.711513791224244,
-0.65));
#9268=CARTESIAN_POINT('Ctrl Pts',(0.375277674973257,0.603180457891261,-0.65));
#9269=CARTESIAN_POINT('Ctrl Pts',(-0.750555349946514,0.603180457891261,
-9.19165206894919E-17));
#9270=CARTESIAN_POINT('Ctrl Pts',(-0.562916512459802,0.711513791224244,
-0.325000000000144));
#9271=CARTESIAN_POINT('Ctrl Pts',(-0.375277674973257,0.603180457891261,
-0.65));
#9272=CARTESIAN_POINT('Origin',(0.375277674973257,0.,-0.65));
#9273=CARTESIAN_POINT('',(-0.375277674973257,0.,-0.65));
#9274=CARTESIAN_POINT('',(0.375277674973257,0.,-0.65));
#9275=CARTESIAN_POINT('Origin',(-0.375277674973257,0.,-0.65));
#9276=CARTESIAN_POINT('',(-0.750555349946514,0.,-9.19165206894919E-17));
#9277=CARTESIAN_POINT('Origin',(-0.750555349946514,0.,-9.19165206894919E-17));
#9278=CARTESIAN_POINT('',(-0.375277674973257,0.,0.65));
#9279=CARTESIAN_POINT('Origin',(0.,0.,0.));
#9280=CARTESIAN_POINT('',(-0.338975,0.68,4.15124648740974E-17));
#9281=CARTESIAN_POINT('Origin',(0.,0.68,0.));
#9282=CARTESIAN_POINT('',(-0.338975,0.,4.15124648740974E-17));
#9283=CARTESIAN_POINT('',(-0.338975,0.,4.15124648740974E-17));
#9284=CARTESIAN_POINT('Origin',(0.,0.,0.));
#9285=CARTESIAN_POINT('Origin',(-0.375277674973257,0.,0.65));
#9286=CARTESIAN_POINT('',(0.375277674973257,0.,0.65));
#9287=CARTESIAN_POINT('Origin',(0.750555349946514,0.,0.));
#9288=CARTESIAN_POINT('',(0.750555349946514,0.,0.));
#9289=CARTESIAN_POINT('Origin',(0.375277674973257,0.,0.65));
#9290=CARTESIAN_POINT('Origin',(0.,0.68,-1.11022302462516E-16));
#9291=CARTESIAN_POINT('Origin',(0.,0.,-1.11022302462516E-16));
#9292=CARTESIAN_POINT('',(0.,0.,0.));
#9293=CARTESIAN_POINT('',(0.,0.,0.));
#9294=CARTESIAN_POINT('Origin',(-1.9,-0.1,4.5));
#9295=CARTESIAN_POINT('',(-2.065,0.,4.5));
#9296=CARTESIAN_POINT('Origin',(-1.9,0.,4.5));
#9297=CARTESIAN_POINT('',(-2.065,1.2,4.5));
#9298=CARTESIAN_POINT('',(-2.065,-0.1,4.5));
#9299=CARTESIAN_POINT('Origin',(-1.9,1.2,4.5));
#9300=CARTESIAN_POINT('Origin',(1.16341445918999E-16,-0.1,6.4));
#9301=CARTESIAN_POINT('',(-0.165,0.,6.4));
#9302=CARTESIAN_POINT('Origin',(1.16341445918999E-16,0.,6.4));
#9303=CARTESIAN_POINT('',(-0.165,1.2,6.4));
#9304=CARTESIAN_POINT('',(-0.165,-0.1,6.4));
#9305=CARTESIAN_POINT('Origin',(1.16341445918999E-16,1.2,6.4));
#9306=CARTESIAN_POINT('Origin',(1.9,-0.1,4.5));
#9307=CARTESIAN_POINT('',(1.735,0.,4.5));
#9308=CARTESIAN_POINT('Origin',(1.9,0.,4.5));
#9309=CARTESIAN_POINT('',(1.735,1.2,4.5));
#9310=CARTESIAN_POINT('',(1.735,-0.1,4.5));
#9311=CARTESIAN_POINT('Origin',(1.9,1.2,4.5));
#9312=CARTESIAN_POINT('Origin',(-3.49024337756996E-16,-0.1,2.6));
#9313=CARTESIAN_POINT('',(-0.165,0.,2.6));
#9314=CARTESIAN_POINT('Origin',(-3.49024337756996E-16,0.,2.6));
#9315=CARTESIAN_POINT('',(-0.165,1.2,2.6));
#9316=CARTESIAN_POINT('',(-0.165,-0.1,2.6));
#9317=CARTESIAN_POINT('Origin',(-3.49024337756996E-16,1.2,2.6));
#9318=CARTESIAN_POINT('Origin',(0.,0.9,4.5));
#9319=CARTESIAN_POINT('',(-1.2,1.2,4.5));
#9320=CARTESIAN_POINT('Origin',(0.,1.2,4.5));
#9321=CARTESIAN_POINT('',(-1.2,0.9,4.5));
#9322=CARTESIAN_POINT('',(-1.2,0.9,4.5));
#9323=CARTESIAN_POINT('Origin',(0.,0.9,4.5));
#9324=CARTESIAN_POINT('Origin',(0.,0.9,4.5));
#9325=CARTESIAN_POINT('',(-1.5,0.9,4.5));
#9326=CARTESIAN_POINT('Origin',(0.,0.9,4.5));
#9327=CARTESIAN_POINT('Origin',(0.,0.,4.5));
#9328=CARTESIAN_POINT('',(-1.5,0.,4.5));
#9329=CARTESIAN_POINT('',(-1.5,0.,4.5));
#9330=CARTESIAN_POINT('Origin',(0.,0.,4.5));
#9331=CARTESIAN_POINT('Origin',(0.,0.,4.5));
#9332=CARTESIAN_POINT('',(-2.2,1.2,4.5));
#9333=CARTESIAN_POINT('Origin',(0.,1.2,4.5));
#9334=CARTESIAN_POINT('',(-2.2,0.,4.5));
#9335=CARTESIAN_POINT('',(-2.2,0.,4.5));
#9336=CARTESIAN_POINT('Origin',(0.,0.,4.5));
#9337=CARTESIAN_POINT('Origin',(0.,1.2,4.5));
#9338=CARTESIAN_POINT('Origin',(0.,0.,4.5));
#9339=CARTESIAN_POINT('',(0.,0.,0.));
#9340=CARTESIAN_POINT('Origin',(-1.9,28.7,4.5));
#9341=CARTESIAN_POINT('',(-2.065,28.8,4.5));
#9342=CARTESIAN_POINT('Origin',(-1.9,28.8,4.5));
#9343=CARTESIAN_POINT('',(-2.065,30.,4.5));
#9344=CARTESIAN_POINT('',(-2.065,28.7,4.5));
#9345=CARTESIAN_POINT('Origin',(-1.9,30.,4.5));
#9346=CARTESIAN_POINT('Origin',(1.16341445918999E-16,28.7,6.4));
#9347=CARTESIAN_POINT('',(-0.165,28.8,6.4));
#9348=CARTESIAN_POINT('Origin',(1.16341445918999E-16,28.8,6.4));
#9349=CARTESIAN_POINT('',(-0.165,30.,6.4));
#9350=CARTESIAN_POINT('',(-0.165,28.7,6.4));
#9351=CARTESIAN_POINT('Origin',(1.16341445918999E-16,30.,6.4));
#9352=CARTESIAN_POINT('Origin',(1.9,28.7,4.5));
#9353=CARTESIAN_POINT('',(1.735,28.8,4.5));
#9354=CARTESIAN_POINT('Origin',(1.9,28.8,4.5));
#9355=CARTESIAN_POINT('',(1.735,30.,4.5));
#9356=CARTESIAN_POINT('',(1.735,28.7,4.5));
#9357=CARTESIAN_POINT('Origin',(1.9,30.,4.5));
#9358=CARTESIAN_POINT('Origin',(-3.49024337756996E-16,28.7,2.6));
#9359=CARTESIAN_POINT('',(-0.165,28.8,2.6));
#9360=CARTESIAN_POINT('Origin',(-3.49024337756996E-16,28.8,2.6));
#9361=CARTESIAN_POINT('',(-0.165,30.,2.6));
#9362=CARTESIAN_POINT('',(-0.165,28.7,2.6));
#9363=CARTESIAN_POINT('Origin',(-3.49024337756996E-16,30.,2.6));
#9364=CARTESIAN_POINT('Origin',(0.,28.8,4.5));
#9365=CARTESIAN_POINT('',(-1.2,29.1,4.5));
#9366=CARTESIAN_POINT('Origin',(0.,29.1,4.5));
#9367=CARTESIAN_POINT('',(-1.2,28.8,4.5));
#9368=CARTESIAN_POINT('',(-1.2,28.8,4.5));
#9369=CARTESIAN_POINT('Origin',(0.,28.8,4.5));
#9370=CARTESIAN_POINT('Origin',(0.,29.1,4.5));
#9371=CARTESIAN_POINT('',(-1.5,29.1,4.5));
#9372=CARTESIAN_POINT('Origin',(0.,29.1,4.5));
#9373=CARTESIAN_POINT('Origin',(0.,28.8,4.5));
#9374=CARTESIAN_POINT('',(-1.5,30.,4.5));
#9375=CARTESIAN_POINT('Origin',(0.,30.,4.5));
#9376=CARTESIAN_POINT('',(-1.5,28.8,4.5));
#9377=CARTESIAN_POINT('Origin',(0.,28.8,4.5));
#9378=CARTESIAN_POINT('',(-2.2,30.,4.5));
#9379=CARTESIAN_POINT('Origin',(0.,30.,4.5));
#9380=CARTESIAN_POINT('',(-2.2,28.8,4.5));
#9381=CARTESIAN_POINT('',(-2.2,28.8,4.5));
#9382=CARTESIAN_POINT('Origin',(0.,28.8,4.5));
#9383=CARTESIAN_POINT('Origin',(0.,30.,4.5));
#9384=CARTESIAN_POINT('Origin',(0.,28.8,4.5));
#9385=CARTESIAN_POINT('',(0.,0.,0.));
#9386=CARTESIAN_POINT('Origin',(0.,0.,4.5));
#9387=CARTESIAN_POINT('',(-2.2,30.,4.5));
#9388=CARTESIAN_POINT('Origin',(0.,30.,4.5));
#9389=CARTESIAN_POINT('',(-2.2,0.,4.5));
#9390=CARTESIAN_POINT('',(-2.2,0.,4.5));
#9391=CARTESIAN_POINT('Origin',(0.,0.,4.5));
#9392=CARTESIAN_POINT('Origin',(0.,0.,4.5));
#9393=CARTESIAN_POINT('',(-2.5,30.,4.5));
#9394=CARTESIAN_POINT('Origin',(0.,30.,4.5));
#9395=CARTESIAN_POINT('',(-2.5,0.,4.5));
#9396=CARTESIAN_POINT('',(-2.5,0.,4.5));
#9397=CARTESIAN_POINT('Origin',(0.,0.,4.5));
#9398=CARTESIAN_POINT('Origin',(0.,30.,4.5));
#9399=CARTESIAN_POINT('Origin',(0.,0.,4.5));
#9400=CARTESIAN_POINT('',(0.,0.,0.));
#9401=CARTESIAN_POINT('Origin',(-1.9,-0.4,4.5));
#9402=CARTESIAN_POINT('',(-2.125,-0.3,4.5));
#9403=CARTESIAN_POINT('Origin',(-1.9,-0.3,4.5));
#9404=CARTESIAN_POINT('',(-2.125,0.,4.5));
#9405=CARTESIAN_POINT('',(-2.125,-0.4,4.5));
#9406=CARTESIAN_POINT('Origin',(-1.9,0.,4.5));
#9407=CARTESIAN_POINT('Origin',(1.16341445918999E-16,-0.4,6.4));
#9408=CARTESIAN_POINT('',(-0.225,-0.3,6.4));
#9409=CARTESIAN_POINT('Origin',(1.16341445918999E-16,-0.3,6.4));
#9410=CARTESIAN_POINT('',(-0.225,0.,6.4));
#9411=CARTESIAN_POINT('',(-0.225,-0.4,6.4));
#9412=CARTESIAN_POINT('Origin',(1.16341445918999E-16,0.,6.4));
#9413=CARTESIAN_POINT('Origin',(1.9,-0.4,4.5));
#9414=CARTESIAN_POINT('',(1.675,-0.3,4.5));
#9415=CARTESIAN_POINT('Origin',(1.9,-0.3,4.5));
#9416=CARTESIAN_POINT('',(1.675,0.,4.5));
#9417=CARTESIAN_POINT('',(1.675,-0.4,4.5));
#9418=CARTESIAN_POINT('Origin',(1.9,0.,4.5));
#9419=CARTESIAN_POINT('Origin',(-3.49024337756996E-16,-0.4,2.6));
#9420=CARTESIAN_POINT('',(-0.225,-0.3,2.6));
#9421=CARTESIAN_POINT('Origin',(-3.49024337756996E-16,-0.3,2.6));
#9422=CARTESIAN_POINT('',(-0.225,0.,2.6));
#9423=CARTESIAN_POINT('',(-0.225,-0.4,2.6));
#9424=CARTESIAN_POINT('Origin',(-3.49024337756996E-16,0.,2.6));
#9425=CARTESIAN_POINT('Origin',(0.,-0.3,4.5));
#9426=CARTESIAN_POINT('',(-1.2,0.,4.5));
#9427=CARTESIAN_POINT('Origin',(0.,0.,4.5));
#9428=CARTESIAN_POINT('',(-1.2,-0.3,4.5));
#9429=CARTESIAN_POINT('',(-1.2,-0.3,4.5));
#9430=CARTESIAN_POINT('Origin',(0.,-0.3,4.5));
#9431=CARTESIAN_POINT('Origin',(0.,-0.3,4.5));
#9432=CARTESIAN_POINT('',(-2.5,0.,4.5));
#9433=CARTESIAN_POINT('Origin',(0.,0.,4.5));
#9434=CARTESIAN_POINT('',(-2.5,-0.3,4.5));
#9435=CARTESIAN_POINT('',(-2.5,-0.3,4.5));
#9436=CARTESIAN_POINT('Origin',(0.,-0.3,4.5));
#9437=CARTESIAN_POINT('Origin',(0.,0.,4.5));
#9438=CARTESIAN_POINT('Origin',(0.,-0.3,4.5));
#9439=CARTESIAN_POINT('',(0.,0.,0.));
#9440=CARTESIAN_POINT('Origin',(0.3,0.4,0.));
#9441=CARTESIAN_POINT('',(-0.3,0.4,-3.67394039744206E-17));
#9442=CARTESIAN_POINT('Origin',(0.,0.4,0.));
#9443=CARTESIAN_POINT('Origin',(0.,0.375,0.));
#9444=CARTESIAN_POINT('',(-0.35,0.35,-4.28626379701573E-17));
#9445=CARTESIAN_POINT('Origin',(0.,0.35,0.));
#9446=CARTESIAN_POINT('',(-0.325,0.375,-3.9801020972289E-17));
#9447=CARTESIAN_POINT('Origin',(0.,0.19,0.));
#9448=CARTESIAN_POINT('',(-0.35,0.03,-4.28626379701574E-17));
#9449=CARTESIAN_POINT('Origin',(0.,0.03,0.));
#9450=CARTESIAN_POINT('',(-0.35,0.19,-4.28626379701574E-17));
#9451=CARTESIAN_POINT('Origin',(0.,0.0149999999999999,0.));
#9452=CARTESIAN_POINT('',(-0.32,-3.29597460435593E-17,-3.91886975727153E-17));
#9453=CARTESIAN_POINT('Origin',(0.,0.,0.));
#9454=CARTESIAN_POINT('',(-0.335,0.0149999999999999,-4.10256677714363E-17));
#9455=CARTESIAN_POINT('Origin',(0.22,0.,0.));
#9456=CARTESIAN_POINT('',(-0.22,-6.93889390390723E-18,-2.69422295812418E-17));
#9457=CARTESIAN_POINT('Origin',(0.,0.,0.));
#9458=CARTESIAN_POINT('Origin',(0.,-0.02,0.));
#9459=CARTESIAN_POINT('',(-0.1954,-0.0492,2.39295984553393E-17));
#9460=CARTESIAN_POINT('Origin',(0.,-0.0492,0.));
#9461=CARTESIAN_POINT('',(-0.21,-0.02,-2.57175827820944E-17));
#9462=CARTESIAN_POINT('Origin',(0.,-0.8,0.));
#9463=CARTESIAN_POINT('',(-0.1954,-1.5646,2.39295984553393E-17));
#9464=CARTESIAN_POINT('Origin',(0.,-1.5646,0.));
#9465=CARTESIAN_POINT('',(-0.1954,-0.8,-2.39295984553393E-17));
#9466=CARTESIAN_POINT('Origin',(0.,-1.58,0.));
#9467=CARTESIAN_POINT('',(-0.16,-1.6,-1.95943487863577E-17));
#9468=CARTESIAN_POINT('Origin',(0.,-1.6,0.));
#9469=CARTESIAN_POINT('',(-0.18,-1.58,-2.20436423846524E-17));
#9470=CARTESIAN_POINT('Origin',(0.,-1.6,0.));
#9471=CARTESIAN_POINT('Origin',(0.0866025403784439,-0.4,-0.15));
#9472=CARTESIAN_POINT('',(0.173205080756888,-0.4,0.));
#9473=CARTESIAN_POINT('',(0.0866025403784439,-0.4,-0.15));
#9474=CARTESIAN_POINT('',(0.173205080756888,-0.4,0.));
#9475=CARTESIAN_POINT('',(0.0866025403784439,-0.64,-0.15));
#9476=CARTESIAN_POINT('',(0.0866025403784439,-0.4,-0.15));
#9477=CARTESIAN_POINT('',(0.173205080756888,-0.64,0.));
#9478=CARTESIAN_POINT('',(0.173205080756888,-0.64,0.));
#9479=CARTESIAN_POINT('',(0.173205080756888,-0.4,0.));
#9480=CARTESIAN_POINT('Origin',(-0.0866025403784438,-0.4,-0.15));
#9481=CARTESIAN_POINT('',(-0.0866025403784438,-0.4,-0.15));
#9482=CARTESIAN_POINT('',(0.0866025403784439,-0.4,-0.15));
#9483=CARTESIAN_POINT('',(-0.0866025403784438,-0.64,-0.15));
#9484=CARTESIAN_POINT('',(-0.0866025403784438,-0.4,-0.15));
#9485=CARTESIAN_POINT('',(0.0866025403784439,-0.64,-0.15));
#9486=CARTESIAN_POINT('Origin',(-0.173205080756888,-0.4,-2.77555756156289E-17));
#9487=CARTESIAN_POINT('',(-0.173205080756888,-0.4,-2.12115047744981E-17));
#9488=CARTESIAN_POINT('',(-0.0866025403784438,-0.4,-0.15));
#9489=CARTESIAN_POINT('',(-0.173205080756888,-0.64,-2.77555756156289E-17));
#9490=CARTESIAN_POINT('',(-0.173205080756888,-0.4,-2.12115047744981E-17));
#9491=CARTESIAN_POINT('',(-0.0866025403784438,-0.64,-0.15));
#9492=CARTESIAN_POINT('Origin',(-0.0866025403784439,-0.4,0.15));
#9493=CARTESIAN_POINT('',(-0.0866025403784439,-0.4,0.15));
#9494=CARTESIAN_POINT('',(-0.173205080756888,-0.4,-2.12115047744981E-17));
#9495=CARTESIAN_POINT('',(-0.0866025403784439,-0.64,0.15));
#9496=CARTESIAN_POINT('',(-0.0866025403784439,-0.4,0.15));
#9497=CARTESIAN_POINT('',(-0.173205080756888,-0.64,-2.12115047744981E-17));
#9498=CARTESIAN_POINT('Origin',(0.0866025403784439,-0.4,0.15));
#9499=CARTESIAN_POINT('',(0.0866025403784439,-0.4,0.15));
#9500=CARTESIAN_POINT('',(-0.0866025403784439,-0.4,0.15));
#9501=CARTESIAN_POINT('',(0.0866025403784439,-0.64,0.15));
#9502=CARTESIAN_POINT('',(0.0866025403784439,-0.4,0.15));
#9503=CARTESIAN_POINT('',(-0.0866025403784439,-0.64,0.15));
#9504=CARTESIAN_POINT('Origin',(0.173205080756888,-0.4,0.));
#9505=CARTESIAN_POINT('',(0.0866025403784439,-0.4,0.15));
#9506=CARTESIAN_POINT('',(0.0866025403784439,-0.64,0.15));
#9507=CARTESIAN_POINT('Origin',(0.,-0.4,-2.77555756156289E-17));
#9508=CARTESIAN_POINT('Origin',(0.,-0.64,-2.77555756156289E-17));
#9509=CARTESIAN_POINT('',(0.,0.,0.));
#9510=CARTESIAN_POINT('',(0.,0.,0.));
#9511=CARTESIAN_POINT('',(0.,0.,0.));
#9512=CARTESIAN_POINT('',(0.,0.,0.));
#9513=CARTESIAN_POINT('',(0.,35.3,0.));
#9514=CARTESIAN_POINT('',(0.,-2.8,4.5));
#9515=CARTESIAN_POINT('',(0.,32.8,4.5));
#9516=CARTESIAN_POINT('',(0.,0.,0.));
#9517=CARTESIAN_POINT('',(0.,34.9,0.));
#9518=CARTESIAN_POINT('',(0.,0.45,4.5));
#9519=CARTESIAN_POINT('',(0.,29.55,4.5));
#9520=CARTESIAN_POINT('',(0.,0.,0.));
#9521=CARTESIAN_POINT('',(0.,0.,0.));
#9522=CARTESIAN_POINT('',(0.,0.,0.));
#9523=CARTESIAN_POINT('',(0.,0.,0.));
#9524=CARTESIAN_POINT('',(-5.,-2.,1.));
#9525=CARTESIAN_POINT('',(-1.5,-2.,1.42));
#9526=CARTESIAN_POINT('',(-1.5,-2.,2.8));
#9527=CARTESIAN_POINT('',(-1.5,-2.,2.9));
#9528=CARTESIAN_POINT('',(1.5,-2.,1.42));
#9529=CARTESIAN_POINT('',(1.5,-2.,2.8));
#9530=CARTESIAN_POINT('',(1.5,-2.,2.9));
#9531=CARTESIAN_POINT('',(-3.5,-2.,1.42));
#9532=CARTESIAN_POINT('',(-3.5,-2.,2.8));
#9533=CARTESIAN_POINT('',(-3.5,-2.,2.9));
#9534=CARTESIAN_POINT('',(-6.2,-2.,4.5));
#9535=CARTESIAN_POINT('',(-5.68,-2.,4.5));
#9536=CARTESIAN_POINT('',(-5.,32.,1.));
#9537=CARTESIAN_POINT('',(-1.5,32.,1.42));
#9538=CARTESIAN_POINT('',(-1.5,32.,2.8));
#9539=CARTESIAN_POINT('',(-1.5,32.,2.9));
#9540=CARTESIAN_POINT('',(1.5,32.,1.42));
#9541=CARTESIAN_POINT('',(1.5,32.,2.8));
#9542=CARTESIAN_POINT('',(1.5,32.,2.9));
#9543=CARTESIAN_POINT('',(-3.5,32.,1.42));
#9544=CARTESIAN_POINT('',(-3.5,32.,2.8));
#9545=CARTESIAN_POINT('',(-3.5,32.,2.9));
#9546=CARTESIAN_POINT('',(-6.2,32.,4.5));
#9547=CARTESIAN_POINT('',(-5.68,32.,4.5));
#9548=CARTESIAN_POINT('',(0.,0.,0.));
#9549=CARTESIAN_POINT('',(0.,0.,0.));
#9550=CARTESIAN_POINT('',(0.,0.,0.));
#9551=CARTESIAN_POINT('',(0.,0.,0.));
#9552=CARTESIAN_POINT('',(1.9,-0.3,4.5));
#9553=CARTESIAN_POINT('',(1.16341445918999E-16,-0.3,6.4));
#9554=CARTESIAN_POINT('',(-1.9,-0.3,4.5));
#9555=CARTESIAN_POINT('',(-3.49024337756996E-16,-0.3,2.6));
#9556=CARTESIAN_POINT('',(0.,30.3,0.));
#9557=CARTESIAN_POINT('',(1.9,30.3,4.5));
#9558=CARTESIAN_POINT('',(1.16341445919E-16,30.3,6.4));
#9559=CARTESIAN_POINT('',(-1.9,30.3,4.5));
#9560=CARTESIAN_POINT('',(-3.49024337756995E-16,30.3,2.6));
#9561=CARTESIAN_POINT('',(0.,0.,0.));
#9562=CARTESIAN_POINT('',(0.,0.,0.));
#9563=UNCERTAINTY_MEASURE_WITH_UNIT(LENGTH_MEASURE(0.001),#9623,
'DISTANCE_ACCURACY_VALUE',
'Maximum model space distance between geometric entities at asserted c
onnectivities');
#9564=UNCERTAINTY_MEASURE_WITH_UNIT(LENGTH_MEASURE(0.001),#9623,
'DISTANCE_ACCURACY_VALUE',
'Maximum model space distance between geometric entities at asserted c
onnectivities');
#9565=UNCERTAINTY_MEASURE_WITH_UNIT(LENGTH_MEASURE(0.001),#9623,
'DISTANCE_ACCURACY_VALUE',
'Maximum model space distance between geometric entities at asserted c
onnectivities');
#9566=UNCERTAINTY_MEASURE_WITH_UNIT(LENGTH_MEASURE(0.001),#9623,
'DISTANCE_ACCURACY_VALUE',
'Maximum model space distance between geometric entities at asserted c
onnectivities');
#9567=UNCERTAINTY_MEASURE_WITH_UNIT(LENGTH_MEASURE(0.001),#9623,
'DISTANCE_ACCURACY_VALUE',
'Maximum model space distance between geometric entities at asserted c
onnectivities');
#9568=UNCERTAINTY_MEASURE_WITH_UNIT(LENGTH_MEASURE(0.001),#9623,
'DISTANCE_ACCURACY_VALUE',
'Maximum model space distance between geometric entities at asserted c
onnectivities');
#9569=UNCERTAINTY_MEASURE_WITH_UNIT(LENGTH_MEASURE(0.001),#9623,
'DISTANCE_ACCURACY_VALUE',
'Maximum model space distance between geometric entities at asserted c
onnectivities');
#9570=UNCERTAINTY_MEASURE_WITH_UNIT(LENGTH_MEASURE(0.001),#9623,
'DISTANCE_ACCURACY_VALUE',
'Maximum model space distance between geometric entities at asserted c
onnectivities');
#9571=UNCERTAINTY_MEASURE_WITH_UNIT(LENGTH_MEASURE(0.001),#9623,
'DISTANCE_ACCURACY_VALUE',
'Maximum model space distance between geometric entities at asserted c
onnectivities');
#9572=UNCERTAINTY_MEASURE_WITH_UNIT(LENGTH_MEASURE(0.001),#9623,
'DISTANCE_ACCURACY_VALUE',
'Maximum model space distance between geometric entities at asserted c
onnectivities');
#9573=UNCERTAINTY_MEASURE_WITH_UNIT(LENGTH_MEASURE(0.001),#9623,
'DISTANCE_ACCURACY_VALUE',
'Maximum model space distance between geometric entities at asserted c
onnectivities');
#9574=UNCERTAINTY_MEASURE_WITH_UNIT(LENGTH_MEASURE(0.001),#9623,
'DISTANCE_ACCURACY_VALUE',
'Maximum model space distance between geometric entities at asserted c
onnectivities');
#9575=UNCERTAINTY_MEASURE_WITH_UNIT(LENGTH_MEASURE(0.001),#9623,
'DISTANCE_ACCURACY_VALUE',
'Maximum model space distance between geometric entities at asserted c
onnectivities');
#9576=UNCERTAINTY_MEASURE_WITH_UNIT(LENGTH_MEASURE(0.001),#9623,
'DISTANCE_ACCURACY_VALUE',
'Maximum model space distance between geometric entities at asserted c
onnectivities');
#9577=UNCERTAINTY_MEASURE_WITH_UNIT(LENGTH_MEASURE(0.001),#9623,
'DISTANCE_ACCURACY_VALUE',
'Maximum model space distance between geometric entities at asserted c
onnectivities');
#9578=UNCERTAINTY_MEASURE_WITH_UNIT(LENGTH_MEASURE(0.001),#9623,
'DISTANCE_ACCURACY_VALUE',
'Maximum model space distance between geometric entities at asserted c
onnectivities');
#9579=UNCERTAINTY_MEASURE_WITH_UNIT(LENGTH_MEASURE(0.001),#9623,
'DISTANCE_ACCURACY_VALUE',
'Maximum model space distance between geometric entities at asserted c
onnectivities');
#9580=UNCERTAINTY_MEASURE_WITH_UNIT(LENGTH_MEASURE(0.001),#9623,
'DISTANCE_ACCURACY_VALUE',
'Maximum model space distance between geometric entities at asserted c
onnectivities');
#9581=UNCERTAINTY_MEASURE_WITH_UNIT(LENGTH_MEASURE(0.001),#9623,
'DISTANCE_ACCURACY_VALUE',
'Maximum model space distance between geometric entities at asserted c
onnectivities');
#9582=UNCERTAINTY_MEASURE_WITH_UNIT(LENGTH_MEASURE(0.001),#9623,
'DISTANCE_ACCURACY_VALUE',
'Maximum model space distance between geometric entities at asserted c
onnectivities');
#9583=UNCERTAINTY_MEASURE_WITH_UNIT(LENGTH_MEASURE(0.001),#9623,
'DISTANCE_ACCURACY_VALUE',
'Maximum model space distance between geometric entities at asserted c
onnectivities');
#9584=UNCERTAINTY_MEASURE_WITH_UNIT(LENGTH_MEASURE(0.001),#9623,
'DISTANCE_ACCURACY_VALUE',
'Maximum model space distance between geometric entities at asserted c
onnectivities');
#9585=UNCERTAINTY_MEASURE_WITH_UNIT(LENGTH_MEASURE(0.001),#9623,
'DISTANCE_ACCURACY_VALUE',
'Maximum model space distance between geometric entities at asserted c
onnectivities');
#9586=UNCERTAINTY_MEASURE_WITH_UNIT(LENGTH_MEASURE(0.001),#9623,
'DISTANCE_ACCURACY_VALUE',
'Maximum model space distance between geometric entities at asserted c
onnectivities');
#9587=UNCERTAINTY_MEASURE_WITH_UNIT(LENGTH_MEASURE(0.001),#9623,
'DISTANCE_ACCURACY_VALUE',
'Maximum model space distance between geometric entities at asserted c
onnectivities');
#9588=UNCERTAINTY_MEASURE_WITH_UNIT(LENGTH_MEASURE(0.001),#9623,
'DISTANCE_ACCURACY_VALUE',
'Maximum model space distance between geometric entities at asserted c
onnectivities');
#9589=UNCERTAINTY_MEASURE_WITH_UNIT(LENGTH_MEASURE(0.001),#9623,
'DISTANCE_ACCURACY_VALUE',
'Maximum model space distance between geometric entities at asserted c
onnectivities');
#9590=UNCERTAINTY_MEASURE_WITH_UNIT(LENGTH_MEASURE(0.001),#9623,
'DISTANCE_ACCURACY_VALUE',
'Maximum model space distance between geometric entities at asserted c
onnectivities');
#9591=UNCERTAINTY_MEASURE_WITH_UNIT(LENGTH_MEASURE(0.001),#9623,
'DISTANCE_ACCURACY_VALUE',
'Maximum model space distance between geometric entities at asserted c
onnectivities');
#9592=UNCERTAINTY_MEASURE_WITH_UNIT(LENGTH_MEASURE(0.001),#9623,
'DISTANCE_ACCURACY_VALUE',
'Maximum model space distance between geometric entities at asserted c
onnectivities');
#9593=(
GEOMETRIC_REPRESENTATION_CONTEXT(3)
GLOBAL_UNCERTAINTY_ASSIGNED_CONTEXT((#9563))
GLOBAL_UNIT_ASSIGNED_CONTEXT((#9623,#9625,#9626))
REPRESENTATION_CONTEXT('','3D')
);
#9594=(
GEOMETRIC_REPRESENTATION_CONTEXT(3)
GLOBAL_UNCERTAINTY_ASSIGNED_CONTEXT((#9564))
GLOBAL_UNIT_ASSIGNED_CONTEXT((#9623,#9625,#9626))
REPRESENTATION_CONTEXT('','3D')
);
#9595=(
GEOMETRIC_REPRESENTATION_CONTEXT(3)
GLOBAL_UNCERTAINTY_ASSIGNED_CONTEXT((#9565))
GLOBAL_UNIT_ASSIGNED_CONTEXT((#9623,#9625,#9626))
REPRESENTATION_CONTEXT('','3D')
);
#9596=(
GEOMETRIC_REPRESENTATION_CONTEXT(3)
GLOBAL_UNCERTAINTY_ASSIGNED_CONTEXT((#9566))
GLOBAL_UNIT_ASSIGNED_CONTEXT((#9623,#9625,#9626))
REPRESENTATION_CONTEXT('','3D')
);
#9597=(
GEOMETRIC_REPRESENTATION_CONTEXT(3)
GLOBAL_UNCERTAINTY_ASSIGNED_CONTEXT((#9567))
GLOBAL_UNIT_ASSIGNED_CONTEXT((#9623,#9625,#9626))
REPRESENTATION_CONTEXT('','3D')
);
#9598=(
GEOMETRIC_REPRESENTATION_CONTEXT(3)
GLOBAL_UNCERTAINTY_ASSIGNED_CONTEXT((#9568))
GLOBAL_UNIT_ASSIGNED_CONTEXT((#9623,#9625,#9626))
REPRESENTATION_CONTEXT('','3D')
);
#9599=(
GEOMETRIC_REPRESENTATION_CONTEXT(3)
GLOBAL_UNCERTAINTY_ASSIGNED_CONTEXT((#9569))
GLOBAL_UNIT_ASSIGNED_CONTEXT((#9623,#9625,#9626))
REPRESENTATION_CONTEXT('','3D')
);
#9600=(
GEOMETRIC_REPRESENTATION_CONTEXT(3)
GLOBAL_UNCERTAINTY_ASSIGNED_CONTEXT((#9570))
GLOBAL_UNIT_ASSIGNED_CONTEXT((#9623,#9625,#9626))
REPRESENTATION_CONTEXT('','3D')
);
#9601=(
GEOMETRIC_REPRESENTATION_CONTEXT(3)
GLOBAL_UNCERTAINTY_ASSIGNED_CONTEXT((#9571))
GLOBAL_UNIT_ASSIGNED_CONTEXT((#9623,#9625,#9626))
REPRESENTATION_CONTEXT('','3D')
);
#9602=(
GEOMETRIC_REPRESENTATION_CONTEXT(3)
GLOBAL_UNCERTAINTY_ASSIGNED_CONTEXT((#9572))
GLOBAL_UNIT_ASSIGNED_CONTEXT((#9623,#9625,#9626))
REPRESENTATION_CONTEXT('','3D')
);
#9603=(
GEOMETRIC_REPRESENTATION_CONTEXT(3)
GLOBAL_UNCERTAINTY_ASSIGNED_CONTEXT((#9573))
GLOBAL_UNIT_ASSIGNED_CONTEXT((#9623,#9625,#9626))
REPRESENTATION_CONTEXT('','3D')
);
#9604=(
GEOMETRIC_REPRESENTATION_CONTEXT(3)
GLOBAL_UNCERTAINTY_ASSIGNED_CONTEXT((#9574))
GLOBAL_UNIT_ASSIGNED_CONTEXT((#9623,#9625,#9626))
REPRESENTATION_CONTEXT('','3D')
);
#9605=(
GEOMETRIC_REPRESENTATION_CONTEXT(3)
GLOBAL_UNCERTAINTY_ASSIGNED_CONTEXT((#9575))
GLOBAL_UNIT_ASSIGNED_CONTEXT((#9623,#9625,#9626))
REPRESENTATION_CONTEXT('','3D')
);
#9606=(
GEOMETRIC_REPRESENTATION_CONTEXT(3)
GLOBAL_UNCERTAINTY_ASSIGNED_CONTEXT((#9576))
GLOBAL_UNIT_ASSIGNED_CONTEXT((#9623,#9625,#9626))
REPRESENTATION_CONTEXT('','3D')
);
#9607=(
GEOMETRIC_REPRESENTATION_CONTEXT(3)
GLOBAL_UNCERTAINTY_ASSIGNED_CONTEXT((#9577))
GLOBAL_UNIT_ASSIGNED_CONTEXT((#9623,#9625,#9626))
REPRESENTATION_CONTEXT('','3D')
);
#9608=(
GEOMETRIC_REPRESENTATION_CONTEXT(3)
GLOBAL_UNCERTAINTY_ASSIGNED_CONTEXT((#9578))
GLOBAL_UNIT_ASSIGNED_CONTEXT((#9623,#9625,#9626))
REPRESENTATION_CONTEXT('','3D')
);
#9609=(
GEOMETRIC_REPRESENTATION_CONTEXT(3)
GLOBAL_UNCERTAINTY_ASSIGNED_CONTEXT((#9579))
GLOBAL_UNIT_ASSIGNED_CONTEXT((#9623,#9625,#9626))
REPRESENTATION_CONTEXT('','3D')
);
#9610=(
GEOMETRIC_REPRESENTATION_CONTEXT(3)
GLOBAL_UNCERTAINTY_ASSIGNED_CONTEXT((#9580))
GLOBAL_UNIT_ASSIGNED_CONTEXT((#9623,#9625,#9626))
REPRESENTATION_CONTEXT('','3D')
);
#9611=(
GEOMETRIC_REPRESENTATION_CONTEXT(3)
GLOBAL_UNCERTAINTY_ASSIGNED_CONTEXT((#9581))
GLOBAL_UNIT_ASSIGNED_CONTEXT((#9623,#9625,#9626))
REPRESENTATION_CONTEXT('','3D')
);
#9612=(
GEOMETRIC_REPRESENTATION_CONTEXT(3)
GLOBAL_UNCERTAINTY_ASSIGNED_CONTEXT((#9582))
GLOBAL_UNIT_ASSIGNED_CONTEXT((#9623,#9625,#9626))
REPRESENTATION_CONTEXT('','3D')
);
#9613=(
GEOMETRIC_REPRESENTATION_CONTEXT(3)
GLOBAL_UNCERTAINTY_ASSIGNED_CONTEXT((#9583))
GLOBAL_UNIT_ASSIGNED_CONTEXT((#9623,#9625,#9626))
REPRESENTATION_CONTEXT('','3D')
);
#9614=(
GEOMETRIC_REPRESENTATION_CONTEXT(3)
GLOBAL_UNCERTAINTY_ASSIGNED_CONTEXT((#9584))
GLOBAL_UNIT_ASSIGNED_CONTEXT((#9623,#9625,#9626))
REPRESENTATION_CONTEXT('','3D')
);
#9615=(
GEOMETRIC_REPRESENTATION_CONTEXT(3)
GLOBAL_UNCERTAINTY_ASSIGNED_CONTEXT((#9585))
GLOBAL_UNIT_ASSIGNED_CONTEXT((#9623,#9625,#9626))
REPRESENTATION_CONTEXT('','3D')
);
#9616=(
GEOMETRIC_REPRESENTATION_CONTEXT(3)
GLOBAL_UNCERTAINTY_ASSIGNED_CONTEXT((#9586))
GLOBAL_UNIT_ASSIGNED_CONTEXT((#9623,#9625,#9626))
REPRESENTATION_CONTEXT('','3D')
);
#9617=(
GEOMETRIC_REPRESENTATION_CONTEXT(3)
GLOBAL_UNCERTAINTY_ASSIGNED_CONTEXT((#9587))
GLOBAL_UNIT_ASSIGNED_CONTEXT((#9623,#9625,#9626))
REPRESENTATION_CONTEXT('','3D')
);
#9618=(
GEOMETRIC_REPRESENTATION_CONTEXT(3)
GLOBAL_UNCERTAINTY_ASSIGNED_CONTEXT((#9588))
GLOBAL_UNIT_ASSIGNED_CONTEXT((#9623,#9625,#9626))
REPRESENTATION_CONTEXT('','3D')
);
#9619=(
GEOMETRIC_REPRESENTATION_CONTEXT(3)
GLOBAL_UNCERTAINTY_ASSIGNED_CONTEXT((#9589))
GLOBAL_UNIT_ASSIGNED_CONTEXT((#9623,#9625,#9626))
REPRESENTATION_CONTEXT('','3D')
);
#9620=(
GEOMETRIC_REPRESENTATION_CONTEXT(3)
GLOBAL_UNCERTAINTY_ASSIGNED_CONTEXT((#9590))
GLOBAL_UNIT_ASSIGNED_CONTEXT((#9623,#9625,#9626))
REPRESENTATION_CONTEXT('','3D')
);
#9621=(
GEOMETRIC_REPRESENTATION_CONTEXT(3)
GLOBAL_UNCERTAINTY_ASSIGNED_CONTEXT((#9591))
GLOBAL_UNIT_ASSIGNED_CONTEXT((#9623,#9625,#9626))
REPRESENTATION_CONTEXT('','3D')
);
#9622=(
GEOMETRIC_REPRESENTATION_CONTEXT(3)
GLOBAL_UNCERTAINTY_ASSIGNED_CONTEXT((#9592))
GLOBAL_UNIT_ASSIGNED_CONTEXT((#9623,#9625,#9626))
REPRESENTATION_CONTEXT('','3D')
);
#9623=(
LENGTH_UNIT()
NAMED_UNIT(*)
SI_UNIT(.CENTI.,.METRE.)
);
#9624=(
LENGTH_UNIT()
NAMED_UNIT(*)
SI_UNIT($,.METRE.)
);
#9625=(
NAMED_UNIT(*)
PLANE_ANGLE_UNIT()
SI_UNIT($,.RADIAN.)
);
#9626=(
NAMED_UNIT(*)
SI_UNIT($,.STERADIAN.)
SOLID_ANGLE_UNIT()
);
#9627=SHAPE_DEFINITION_REPRESENTATION(#9656,#9744);
#9628=SHAPE_DEFINITION_REPRESENTATION(#9657,#9745);
#9629=SHAPE_DEFINITION_REPRESENTATION(#9658,#9746);
#9630=SHAPE_DEFINITION_REPRESENTATION(#9659,#9747);
#9631=SHAPE_DEFINITION_REPRESENTATION(#9660,#9748);
#9632=SHAPE_DEFINITION_REPRESENTATION(#9661,#9749);
#9633=SHAPE_DEFINITION_REPRESENTATION(#9662,#9750);
#9634=SHAPE_DEFINITION_REPRESENTATION(#9663,#9751);
#9635=SHAPE_DEFINITION_REPRESENTATION(#9664,#9752);
#9636=SHAPE_DEFINITION_REPRESENTATION(#9665,#9753);
#9637=SHAPE_DEFINITION_REPRESENTATION(#9666,#9754);
#9638=SHAPE_DEFINITION_REPRESENTATION(#9667,#9755);
#9639=SHAPE_DEFINITION_REPRESENTATION(#9668,#9756);
#9640=SHAPE_DEFINITION_REPRESENTATION(#9674,#9757);
#9641=SHAPE_DEFINITION_REPRESENTATION(#9675,#9758);
#9642=SHAPE_DEFINITION_REPRESENTATION(#9676,#9759);
#9643=SHAPE_DEFINITION_REPRESENTATION(#9677,#9760);
#9644=SHAPE_DEFINITION_REPRESENTATION(#9678,#9761);
#9645=SHAPE_DEFINITION_REPRESENTATION(#9679,#9762);
#9646=SHAPE_DEFINITION_REPRESENTATION(#9680,#9763);
#9647=SHAPE_DEFINITION_REPRESENTATION(#9681,#9764);
#9648=SHAPE_DEFINITION_REPRESENTATION(#9682,#9765);
#9649=SHAPE_DEFINITION_REPRESENTATION(#9683,#9766);
#9650=SHAPE_DEFINITION_REPRESENTATION(#9684,#9767);
#9651=SHAPE_DEFINITION_REPRESENTATION(#9685,#9768);
#9652=SHAPE_DEFINITION_REPRESENTATION(#9686,#9769);
#9653=SHAPE_DEFINITION_REPRESENTATION(#9687,#9770);
#9654=SHAPE_DEFINITION_REPRESENTATION(#9688,#9771);
#9655=SHAPE_DEFINITION_REPRESENTATION(#9689,#9772);
#9656=PRODUCT_DEFINITION_SHAPE('',$,#9774);
#9657=PRODUCT_DEFINITION_SHAPE('',$,#9775);
#9658=PRODUCT_DEFINITION_SHAPE('',$,#9776);
#9659=PRODUCT_DEFINITION_SHAPE('',$,#9777);
#9660=PRODUCT_DEFINITION_SHAPE('',$,#9778);
#9661=PRODUCT_DEFINITION_SHAPE('',$,#9779);
#9662=PRODUCT_DEFINITION_SHAPE('',$,#9780);
#9663=PRODUCT_DEFINITION_SHAPE('',$,#9781);
#9664=PRODUCT_DEFINITION_SHAPE('',$,#9782);
#9665=PRODUCT_DEFINITION_SHAPE('',$,#9783);
#9666=PRODUCT_DEFINITION_SHAPE('',$,#9784);
#9667=PRODUCT_DEFINITION_SHAPE('',$,#9785);
#9668=PRODUCT_DEFINITION_SHAPE('',$,#9786);
#9669=PRODUCT_DEFINITION_SHAPE($,$,#212);
#9670=PRODUCT_DEFINITION_SHAPE($,$,#213);
#9671=PRODUCT_DEFINITION_SHAPE($,$,#214);
#9672=PRODUCT_DEFINITION_SHAPE($,$,#215);
#9673=PRODUCT_DEFINITION_SHAPE($,$,#216);
#9674=PRODUCT_DEFINITION_SHAPE('',$,#9787);
#9675=PRODUCT_DEFINITION_SHAPE('',$,#9788);
#9676=PRODUCT_DEFINITION_SHAPE('',$,#9789);
#9677=PRODUCT_DEFINITION_SHAPE('',$,#9790);
#9678=PRODUCT_DEFINITION_SHAPE('',$,#9791);
#9679=PRODUCT_DEFINITION_SHAPE('',$,#9792);
#9680=PRODUCT_DEFINITION_SHAPE('',$,#9793);
#9681=PRODUCT_DEFINITION_SHAPE('',$,#9794);
#9682=PRODUCT_DEFINITION_SHAPE('',$,#9795);
#9683=PRODUCT_DEFINITION_SHAPE('',$,#9796);
#9684=PRODUCT_DEFINITION_SHAPE('',$,#9797);
#9685=PRODUCT_DEFINITION_SHAPE('',$,#9798);
#9686=PRODUCT_DEFINITION_SHAPE('',$,#9799);
#9687=PRODUCT_DEFINITION_SHAPE('',$,#9800);
#9688=PRODUCT_DEFINITION_SHAPE('',$,#9801);
#9689=PRODUCT_DEFINITION_SHAPE('',$,#9802);
#9690=PRODUCT_DEFINITION_SHAPE($,$,#217);
#9691=PRODUCT_DEFINITION_SHAPE($,$,#218);
#9692=PRODUCT_DEFINITION_SHAPE($,$,#219);
#9693=PRODUCT_DEFINITION_SHAPE($,$,#220);
#9694=PRODUCT_DEFINITION_SHAPE($,$,#221);
#9695=PRODUCT_DEFINITION_SHAPE($,$,#222);
#9696=PRODUCT_DEFINITION_SHAPE($,$,#223);
#9697=PRODUCT_DEFINITION_SHAPE($,$,#224);
#9698=PRODUCT_DEFINITION_SHAPE($,$,#225);
#9699=PRODUCT_DEFINITION_SHAPE($,$,#226);
#9700=PRODUCT_DEFINITION_SHAPE($,$,#227);
#9701=PRODUCT_DEFINITION_SHAPE($,$,#228);
#9702=PRODUCT_DEFINITION_SHAPE($,$,#229);
#9703=PRODUCT_DEFINITION_SHAPE($,$,#230);
#9704=PRODUCT_DEFINITION_SHAPE($,$,#231);
#9705=PRODUCT_DEFINITION_SHAPE($,$,#232);
#9706=PRODUCT_DEFINITION_SHAPE($,$,#233);
#9707=PRODUCT_DEFINITION_SHAPE($,$,#234);
#9708=PRODUCT_DEFINITION_SHAPE($,$,#235);
#9709=PRODUCT_DEFINITION_SHAPE($,$,#236);
#9710=PRODUCT_DEFINITION_SHAPE($,$,#237);
#9711=PRODUCT_DEFINITION_SHAPE($,$,#238);
#9712=PRODUCT_DEFINITION_SHAPE($,$,#239);
#9713=PRODUCT_DEFINITION_SHAPE($,$,#240);
#9714=PRODUCT_DEFINITION_SHAPE($,$,#241);
#9715=PRODUCT_DEFINITION_SHAPE($,$,#242);
#9716=PRODUCT_DEFINITION_SHAPE($,$,#243);
#9717=PRODUCT_DEFINITION_SHAPE($,$,#244);
#9718=PRODUCT_DEFINITION_SHAPE($,$,#245);
#9719=PRODUCT_DEFINITION_SHAPE($,$,#246);
#9720=PRODUCT_DEFINITION_SHAPE($,$,#247);
#9721=PRODUCT_DEFINITION_SHAPE($,$,#248);
#9722=PRODUCT_DEFINITION_SHAPE($,$,#249);
#9723=PRODUCT_DEFINITION_SHAPE($,$,#250);
#9724=PRODUCT_DEFINITION_SHAPE($,$,#251);
#9725=PRODUCT_DEFINITION_SHAPE($,$,#252);
#9726=PRODUCT_DEFINITION_SHAPE($,$,#253);
#9727=PRODUCT_DEFINITION_SHAPE($,$,#254);
#9728=PRODUCT_DEFINITION_SHAPE($,$,#255);
#9729=PRODUCT_DEFINITION_SHAPE($,$,#256);
#9730=PRODUCT_DEFINITION_SHAPE($,$,#257);
#9731=PRODUCT_DEFINITION_SHAPE($,$,#258);
#9732=PRODUCT_DEFINITION_SHAPE($,$,#259);
#9733=PRODUCT_DEFINITION_SHAPE($,$,#260);
#9734=PRODUCT_DEFINITION_SHAPE($,$,#261);
#9735=PRODUCT_DEFINITION_SHAPE($,$,#262);
#9736=PRODUCT_DEFINITION_SHAPE($,$,#263);
#9737=PRODUCT_DEFINITION_SHAPE($,$,#264);
#9738=PRODUCT_DEFINITION_SHAPE($,$,#265);
#9739=PRODUCT_DEFINITION_SHAPE($,$,#266);
#9740=PRODUCT_DEFINITION_SHAPE($,$,#267);
#9741=PRODUCT_DEFINITION_SHAPE($,$,#268);
#9742=PRODUCT_DEFINITION_SHAPE($,$,#269);
#9743=PRODUCT_DEFINITION_SHAPE($,$,#270);
#9744=SHAPE_REPRESENTATION('',(#5509,#6105,#6106),#9593);
#9745=SHAPE_REPRESENTATION('',(#5510,#6053,#6054,#6055,#6056,#6057,#6058,
#6059,#6060,#6061,#6062,#6063,#6064,#6065,#6066,#6067,#6068,#6069,#6070,
#6071,#6072,#6073,#6074,#6075,#6076,#6077,#6078,#6079,#6080,#6081,#6082,
#6083,#6084,#6085,#6086,#6087,#6088,#6089,#6090,#6091),#9594);
#9746=SHAPE_REPRESENTATION('',(#5511),#9595);
#9747=SHAPE_REPRESENTATION('',(#5533),#9596);
#9748=SHAPE_REPRESENTATION('',(#5542),#9597);
#9749=SHAPE_REPRESENTATION('',(#5551),#9598);
#9750=SHAPE_REPRESENTATION('',(#5560),#9599);
#9751=SHAPE_REPRESENTATION('',(#5569,#5698,#5699,#5700,#5701,#5702),#9600);
#9752=SHAPE_REPRESENTATION('',(#5570),#9601);
#9753=SHAPE_REPRESENTATION('',(#5590),#9602);
#9754=SHAPE_REPRESENTATION('',(#5610),#9603);
#9755=SHAPE_REPRESENTATION('',(#5627),#9604);
#9756=SHAPE_REPRESENTATION('',(#5681),#9605);
#9757=SHAPE_REPRESENTATION('',(#5703),#9606);
#9758=SHAPE_REPRESENTATION('',(#5742),#9607);
#9759=SHAPE_REPRESENTATION('',(#5757),#9608);
#9760=SHAPE_REPRESENTATION('',(#5796),#9609);
#9761=SHAPE_REPRESENTATION('',(#5811),#9610);
#9762=SHAPE_REPRESENTATION('',(#5861),#9611);
#9763=SHAPE_REPRESENTATION('',(#5878),#9612);
#9764=SHAPE_REPRESENTATION('',(#5889),#9613);
#9765=SHAPE_REPRESENTATION('',(#5913),#9614);
#9766=SHAPE_REPRESENTATION('',(#5930),#9615);
#9767=SHAPE_REPRESENTATION('',(#5946,#6092,#6093,#6094,#6095,#6096,#6097,
#6098,#6099,#6100,#6101,#6102,#6103,#6104),#9616);
#9768=SHAPE_REPRESENTATION('',(#5947),#9617);
#9769=SHAPE_REPRESENTATION('',(#5972),#9618);
#9770=SHAPE_REPRESENTATION('',(#5997),#9619);
#9771=SHAPE_REPRESENTATION('',(#6006),#9620);
#9772=SHAPE_REPRESENTATION('',(#6027),#9621);
#9773=PRODUCT_DEFINITION_CONTEXT('part definition',#9862,'design');
#9774=PRODUCT_DEFINITION('PAT-001',
'PAT-001',#9803,#9773);
#9775=PRODUCT_DEFINITION('Axle brackets and bearings',
'Axle brackets and bearings',#9804,#9773);
#9776=PRODUCT_DEFINITION('Stepped axle','Stepped axle',#9805,#9773);
#9777=PRODUCT_DEFINITION('Journal spacer','Journal spacer',#9806,#9773);
#9778=PRODUCT_DEFINITION('Journal spacer (1)','Journal spacer (1)',#9807,
#9773);
#9779=PRODUCT_DEFINITION('End keeper','End keeper',#9808,#9773);
#9780=PRODUCT_DEFINITION('Bracket shim','Bracket shim',#9809,#9773);
#9781=PRODUCT_DEFINITION('Cleared radial bearing',
'Cleared radial bearing',#9810,#9773);
#9782=PRODUCT_DEFINITION('Inner ring','Inner ring',#9811,#9773);
#9783=PRODUCT_DEFINITION('Outer ring','Outer ring',#9812,#9773);
#9784=PRODUCT_DEFINITION('Balls','Balls',#9813,#9773);
#9785=PRODUCT_DEFINITION('Cage','Cage',#9814,#9773);
#9786=PRODUCT_DEFINITION('Seals 2RS','Seals 2RS',#9815,#9773);
#9787=PRODUCT_DEFINITION('Sliding axle block','Sliding axle block',#9816,
#9773);
#9788=PRODUCT_DEFINITION('Take-up screw bracket',
'Take-up screw bracket',#9817,#9773);
#9789=PRODUCT_DEFINITION('Sliding axle block (1)',
'Sliding axle block (1)',#9818,#9773);
#9790=PRODUCT_DEFINITION('Take-up screw bracket (1)',
'Take-up screw bracket (1)',#9819,#9773);
#9791=PRODUCT_DEFINITION('Slotted Extrusion - 20 x 20 x 100 mm',
'Slotted Extrusion - 20 x 20 x 100 mm',#9820,#9773);
#9792=PRODUCT_DEFINITION('Slot Nut - M5 for 20 mm Extrusion',
'Slot Nut - M5 for 20 mm Extrusion',#9821,#9773);
#9793=PRODUCT_DEFINITION('Flat Washer - M5','Flat Washer - M5',#9822,#9773);
#9794=PRODUCT_DEFINITION('M5x14 Cap Screw','M5x14 Cap Screw',#9823,#9773);
#9795=PRODUCT_DEFINITION('Hex Bolt - M8x40','Hex Bolt - M8x40',#9824,#9773);
#9796=PRODUCT_DEFINITION('Hex Nut - M8','Hex Nut - M8',#9825,#9773);
#9797=PRODUCT_DEFINITION('Roller tube and end caps',
'Roller tube and end caps',#9826,#9773);
#9798=PRODUCT_DEFINITION('Bearing insert','Bearing insert',#9827,#9773);
#9799=PRODUCT_DEFINITION('Bearing insert (1)','Bearing insert (1)',#9828,
#9773);
#9800=PRODUCT_DEFINITION('Roller tube','Roller tube',#9829,#9773);
#9801=PRODUCT_DEFINITION('Outer race retainer','Outer race retainer',#9830,
#9773);
#9802=PRODUCT_DEFINITION('Cap Screw - M4x16','Cap Screw - M4x16',#9831,
#9773);
#9803=PRODUCT_DEFINITION_FORMATION('',$,#9864);
#9804=PRODUCT_DEFINITION_FORMATION('',$,#9865);
#9805=PRODUCT_DEFINITION_FORMATION('',$,#9866);
#9806=PRODUCT_DEFINITION_FORMATION('',$,#9867);
#9807=PRODUCT_DEFINITION_FORMATION('',$,#9868);
#9808=PRODUCT_DEFINITION_FORMATION('',$,#9869);
#9809=PRODUCT_DEFINITION_FORMATION('',$,#9870);
#9810=PRODUCT_DEFINITION_FORMATION('',$,#9871);
#9811=PRODUCT_DEFINITION_FORMATION('',$,#9872);
#9812=PRODUCT_DEFINITION_FORMATION('',$,#9873);
#9813=PRODUCT_DEFINITION_FORMATION('',$,#9874);
#9814=PRODUCT_DEFINITION_FORMATION('',$,#9875);
#9815=PRODUCT_DEFINITION_FORMATION('',$,#9876);
#9816=PRODUCT_DEFINITION_FORMATION('',$,#9877);
#9817=PRODUCT_DEFINITION_FORMATION('',$,#9878);
#9818=PRODUCT_DEFINITION_FORMATION('',$,#9879);
#9819=PRODUCT_DEFINITION_FORMATION('',$,#9880);
#9820=PRODUCT_DEFINITION_FORMATION('',$,#9881);
#9821=PRODUCT_DEFINITION_FORMATION('',$,#9882);
#9822=PRODUCT_DEFINITION_FORMATION('',$,#9883);
#9823=PRODUCT_DEFINITION_FORMATION('',$,#9884);
#9824=PRODUCT_DEFINITION_FORMATION('',$,#9885);
#9825=PRODUCT_DEFINITION_FORMATION('',$,#9886);
#9826=PRODUCT_DEFINITION_FORMATION('',$,#9887);
#9827=PRODUCT_DEFINITION_FORMATION('',$,#9888);
#9828=PRODUCT_DEFINITION_FORMATION('',$,#9889);
#9829=PRODUCT_DEFINITION_FORMATION('',$,#9890);
#9830=PRODUCT_DEFINITION_FORMATION('',$,#9891);
#9831=PRODUCT_DEFINITION_FORMATION('',$,#9892);
#9832=PRODUCT_RELATED_PRODUCT_CATEGORY('PAT-001',
'PAT-001',(#9864));
#9833=PRODUCT_RELATED_PRODUCT_CATEGORY('Axle brackets and bearings',
'Axle brackets and bearings',(#9865));
#9834=PRODUCT_RELATED_PRODUCT_CATEGORY('Stepped axle','Stepped axle',(#9866));
#9835=PRODUCT_RELATED_PRODUCT_CATEGORY('Journal spacer',
'Journal spacer',(#9867));
#9836=PRODUCT_RELATED_PRODUCT_CATEGORY('Journal spacer (1)',
'Journal spacer (1)',(#9868));
#9837=PRODUCT_RELATED_PRODUCT_CATEGORY('End keeper','End keeper',(#9869));
#9838=PRODUCT_RELATED_PRODUCT_CATEGORY('Bracket shim','Bracket shim',(#9870));
#9839=PRODUCT_RELATED_PRODUCT_CATEGORY('Cleared radial bearing',
'Cleared radial bearing',(#9871));
#9840=PRODUCT_RELATED_PRODUCT_CATEGORY('Inner ring','Inner ring',(#9872));
#9841=PRODUCT_RELATED_PRODUCT_CATEGORY('Outer ring','Outer ring',(#9873));
#9842=PRODUCT_RELATED_PRODUCT_CATEGORY('Balls','Balls',(#9874));
#9843=PRODUCT_RELATED_PRODUCT_CATEGORY('Cage','Cage',(#9875));
#9844=PRODUCT_RELATED_PRODUCT_CATEGORY('Seals 2RS','Seals 2RS',(#9876));
#9845=PRODUCT_RELATED_PRODUCT_CATEGORY('Sliding axle block',
'Sliding axle block',(#9877));
#9846=PRODUCT_RELATED_PRODUCT_CATEGORY('Take-up screw bracket',
'Take-up screw bracket',(#9878));
#9847=PRODUCT_RELATED_PRODUCT_CATEGORY('Sliding axle block (1)',
'Sliding axle block (1)',(#9879));
#9848=PRODUCT_RELATED_PRODUCT_CATEGORY('Take-up screw bracket (1)',
'Take-up screw bracket (1)',(#9880));
#9849=PRODUCT_RELATED_PRODUCT_CATEGORY(
'Slotted Extrusion - 20 x 20 x 100 mm',
'Slotted Extrusion - 20 x 20 x 100 mm',(#9881));
#9850=PRODUCT_RELATED_PRODUCT_CATEGORY(
'Slot Nut - M5 for 20 mm Extrusion','Slot Nut - M5 for 20 mm Extrusion',
(#9882));
#9851=PRODUCT_RELATED_PRODUCT_CATEGORY('Flat Washer - M5',
'Flat Washer - M5',(#9883));
#9852=PRODUCT_RELATED_PRODUCT_CATEGORY('M5x14 Cap Screw',
'M5x14 Cap Screw',(#9884));
#9853=PRODUCT_RELATED_PRODUCT_CATEGORY('Hex Bolt - M8x40',
'Hex Bolt - M8x40',(#9885));
#9854=PRODUCT_RELATED_PRODUCT_CATEGORY('Hex Nut - M8','Hex Nut - M8',(#9886));
#9855=PRODUCT_RELATED_PRODUCT_CATEGORY('Roller tube and end caps',
'Roller tube and end caps',(#9887));
#9856=PRODUCT_RELATED_PRODUCT_CATEGORY('Bearing insert',
'Bearing insert',(#9888));
#9857=PRODUCT_RELATED_PRODUCT_CATEGORY('Bearing insert (1)',
'Bearing insert (1)',(#9889));
#9858=PRODUCT_RELATED_PRODUCT_CATEGORY('Roller tube','Roller tube',(#9890));
#9859=PRODUCT_RELATED_PRODUCT_CATEGORY('Outer race retainer',
'Outer race retainer',(#9891));
#9860=PRODUCT_RELATED_PRODUCT_CATEGORY('Cap Screw - M4x16',
'Cap Screw - M4x16',(#9892));
#9861=APPLICATION_PROTOCOL_DEFINITION('international standard',
'automotive_design',2009,#9862);
#9862=APPLICATION_CONTEXT(
'Core Data for Automotive Mechanical Design Process');
#9863=PRODUCT_CONTEXT('part definition',#9862,'mechanical');
#9864=PRODUCT('PAT-001',
'PAT-001','PAT-001',(#9863));
#9865=PRODUCT('Axle brackets and bearings','Axle brackets and bearings',
'Axle brackets and bearings',(#9863));
#9866=PRODUCT('Stepped axle','Stepped axle','Stepped axle',(#9863));
#9867=PRODUCT('Journal spacer','Journal spacer','Journal spacer',(#9863));
#9868=PRODUCT('Journal spacer (1)','Journal spacer (1)','Journal spacer (1)',
(#9863));
#9869=PRODUCT('End keeper','End keeper','End keeper',(#9863));
#9870=PRODUCT('Bracket shim','Bracket shim','Bracket shim',(#9863));
#9871=PRODUCT('Cleared radial bearing','Cleared radial bearing',
'Cleared radial bearing',(#9863));
#9872=PRODUCT('Inner ring','Inner ring','Inner ring',(#9863));
#9873=PRODUCT('Outer ring','Outer ring','Outer ring',(#9863));
#9874=PRODUCT('Balls','Balls','Balls',(#9863));
#9875=PRODUCT('Cage','Cage','Cage',(#9863));
#9876=PRODUCT('Seals 2RS','Seals 2RS','Seals 2RS',(#9863));
#9877=PRODUCT('Sliding axle block','Sliding axle block',
'Sliding axle block',(#9863));
#9878=PRODUCT('Take-up screw bracket','Take-up screw bracket',
'Take-up screw bracket',(#9863));
#9879=PRODUCT('Sliding axle block (1)','Sliding axle block (1)',
'Sliding axle block (1)',(#9863));
#9880=PRODUCT('Take-up screw bracket (1)','Take-up screw bracket (1)',
'Take-up screw bracket (1)',(#9863));
#9881=PRODUCT('Slotted Extrusion - 20 x 20 x 100 mm',
'Slotted Extrusion - 20 x 20 x 100 mm',
'Slotted Extrusion - 20 x 20 x 100 mm',(#9863));
#9882=PRODUCT('Slot Nut - M5 for 20 mm Extrusion',
'Slot Nut - M5 for 20 mm Extrusion','Slot Nut - M5 for 20 mm Extrusion',
(#9863));
#9883=PRODUCT('Flat Washer - M5','Flat Washer - M5','Flat Washer - M5',
(#9863));
#9884=PRODUCT('M5x14 Cap Screw','M5x14 Cap Screw','M5x14 Cap Screw',(#9863));
#9885=PRODUCT('Hex Bolt - M8x40','Hex Bolt - M8x40','Hex Bolt - M8x40',
(#9863));
#9886=PRODUCT('Hex Nut - M8','Hex Nut - M8','Hex Nut - M8',(#9863));
#9887=PRODUCT('Roller tube and end caps','Roller tube and end caps',
'Roller tube and end caps',(#9863));
#9888=PRODUCT('Bearing insert','Bearing insert','Bearing insert',(#9863));
#9889=PRODUCT('Bearing insert (1)','Bearing insert (1)','Bearing insert (1)',
(#9863));
#9890=PRODUCT('Roller tube','Roller tube','Roller tube',(#9863));
#9891=PRODUCT('Outer race retainer','Outer race retainer',
'Outer race retainer',(#9863));
#9892=PRODUCT('Cap Screw - M4x16','Cap Screw - M4x16',
'Cap Screw - M4x16',(#9863));
#9893=PRESENTATION_STYLE_ASSIGNMENT((#9899));
#9894=PRESENTATION_STYLE_ASSIGNMENT((#9900));
#9895=PRESENTATION_STYLE_ASSIGNMENT((#9901));
#9896=PRESENTATION_STYLE_ASSIGNMENT((#9902));
#9897=PRESENTATION_STYLE_ASSIGNMENT((#9903));
#9898=PRESENTATION_STYLE_ASSIGNMENT((#9904));
#9899=SURFACE_STYLE_USAGE(.BOTH.,#9905);
#9900=SURFACE_STYLE_USAGE(.BOTH.,#9906);
#9901=SURFACE_STYLE_USAGE(.BOTH.,#9907);
#9902=SURFACE_STYLE_USAGE(.BOTH.,#9908);
#9903=SURFACE_STYLE_USAGE(.BOTH.,#9909);
#9904=SURFACE_STYLE_USAGE(.BOTH.,#9910);
#9905=SURFACE_SIDE_STYLE('',(#9911));
#9906=SURFACE_SIDE_STYLE('',(#9912));
#9907=SURFACE_SIDE_STYLE('',(#9913));
#9908=SURFACE_SIDE_STYLE('',(#9914));
#9909=SURFACE_SIDE_STYLE('',(#9915));
#9910=SURFACE_SIDE_STYLE('',(#9916));
#9911=SURFACE_STYLE_FILL_AREA(#9917);
#9912=SURFACE_STYLE_FILL_AREA(#9918);
#9913=SURFACE_STYLE_FILL_AREA(#9919);
#9914=SURFACE_STYLE_FILL_AREA(#9920);
#9915=SURFACE_STYLE_FILL_AREA(#9921);
#9916=SURFACE_STYLE_FILL_AREA(#9922);
#9917=FILL_AREA_STYLE('Steel - Satin',(#9923));
#9918=FILL_AREA_STYLE('CAD Library Painted - Engineering blue',(#9924));
#9919=FILL_AREA_STYLE('CAD Library Painted - Steel gray',(#9925));
#9920=FILL_AREA_STYLE('CAD Library Painted - Off white',(#9926));
#9921=FILL_AREA_STYLE('CAD Library Painted - Light blue',(#9927));
#9922=FILL_AREA_STYLE('CAD Library Painted - Graphite',(#9928));
#9923=FILL_AREA_STYLE_COLOUR('Steel - Satin',#9929);
#9924=FILL_AREA_STYLE_COLOUR('CAD Library Painted - Engineering blue',#9930);
#9925=FILL_AREA_STYLE_COLOUR('CAD Library Painted - Steel gray',#9931);
#9926=FILL_AREA_STYLE_COLOUR('CAD Library Painted - Off white',#9932);
#9927=FILL_AREA_STYLE_COLOUR('CAD Library Painted - Light blue',#9933);
#9928=FILL_AREA_STYLE_COLOUR('CAD Library Painted - Graphite',#9934);
#9929=COLOUR_RGB('Steel - Satin',0.627450980392157,0.627450980392157,0.627450980392157);
#9930=COLOUR_RGB('CAD Library Painted - Engineering blue',0.12156862745098,
0.356862745098039,0.6);
#9931=COLOUR_RGB('CAD Library Painted - Steel gray',0.592156862745098,0.631372549019608,
0.67843137254902);
#9932=COLOUR_RGB('CAD Library Painted - Off white',0.909803921568627,0.901960784313726,
0.858823529411765);
#9933=COLOUR_RGB('CAD Library Painted - Light blue',0.286274509803922,0.552941176470588,
0.780392156862745);
#9934=COLOUR_RGB('CAD Library Painted - Graphite',0.0980392156862745,0.109803921568627,
0.125490196078431);
#9935=COLOUR_RGB('Dark Blue',0.08,0.2,0.34);
#9936=FILL_AREA_STYLE_COLOUR('',#9935);
#9937=FILL_AREA_STYLE('',(#9936));
#9938=SURFACE_STYLE_FILL_AREA(#9937);
#9939=SURFACE_SIDE_STYLE('',(#9938));
#9940=SURFACE_STYLE_USAGE(.BOTH.,#9939);
#9941=PRESENTATION_STYLE_ASSIGNMENT((#9940));
#9942=COLOUR_RGB('Light Blue',0.38,0.62,0.78);
#9943=FILL_AREA_STYLE_COLOUR('',#9942);
#9944=FILL_AREA_STYLE('',(#9943));
#9945=SURFACE_STYLE_FILL_AREA(#9944);
#9946=SURFACE_SIDE_STYLE('',(#9945));
#9947=SURFACE_STYLE_USAGE(.BOTH.,#9946);
#9948=PRESENTATION_STYLE_ASSIGNMENT((#9947));
#9949=COLOUR_RGB('Sky Blue',0.24,0.69,0.87);
#9950=FILL_AREA_STYLE_COLOUR('',#9949);
#9951=FILL_AREA_STYLE('',(#9950));
#9952=SURFACE_STYLE_FILL_AREA(#9951);
#9953=SURFACE_SIDE_STYLE('',(#9952));
#9954=SURFACE_STYLE_USAGE(.BOTH.,#9953);
#9955=PRESENTATION_STYLE_ASSIGNMENT((#9954));
#9956=COLOUR_RGB('Grey',0.48,0.52,0.57);
#9957=FILL_AREA_STYLE_COLOUR('',#9956);
#9958=FILL_AREA_STYLE('',(#9957));
#9959=SURFACE_STYLE_FILL_AREA(#9958);
#9960=SURFACE_SIDE_STYLE('',(#9959));
#9961=SURFACE_STYLE_USAGE(.BOTH.,#9960);
#9962=PRESENTATION_STYLE_ASSIGNMENT((#9961));
#9963=COLOUR_RGB('Black',0.12,0.14,0.17);
#9964=FILL_AREA_STYLE_COLOUR('',#9963);
#9965=FILL_AREA_STYLE('',(#9964));
#9966=SURFACE_STYLE_FILL_AREA(#9965);
#9967=SURFACE_SIDE_STYLE('',(#9966));
#9968=SURFACE_STYLE_USAGE(.BOTH.,#9967);
#9969=PRESENTATION_STYLE_ASSIGNMENT((#9968));
#9970=COLOUR_RGB('Off White',0.89,0.88,0.83);
#9971=FILL_AREA_STYLE_COLOUR('',#9970);
#9972=FILL_AREA_STYLE('',(#9971));
#9973=SURFACE_STYLE_FILL_AREA(#9972);
#9974=SURFACE_SIDE_STYLE('',(#9973));
#9975=SURFACE_STYLE_USAGE(.BOTH.,#9974);
#9976=PRESENTATION_STYLE_ASSIGNMENT((#9975));
ENDSEC;
END-ISO-10303-21;
